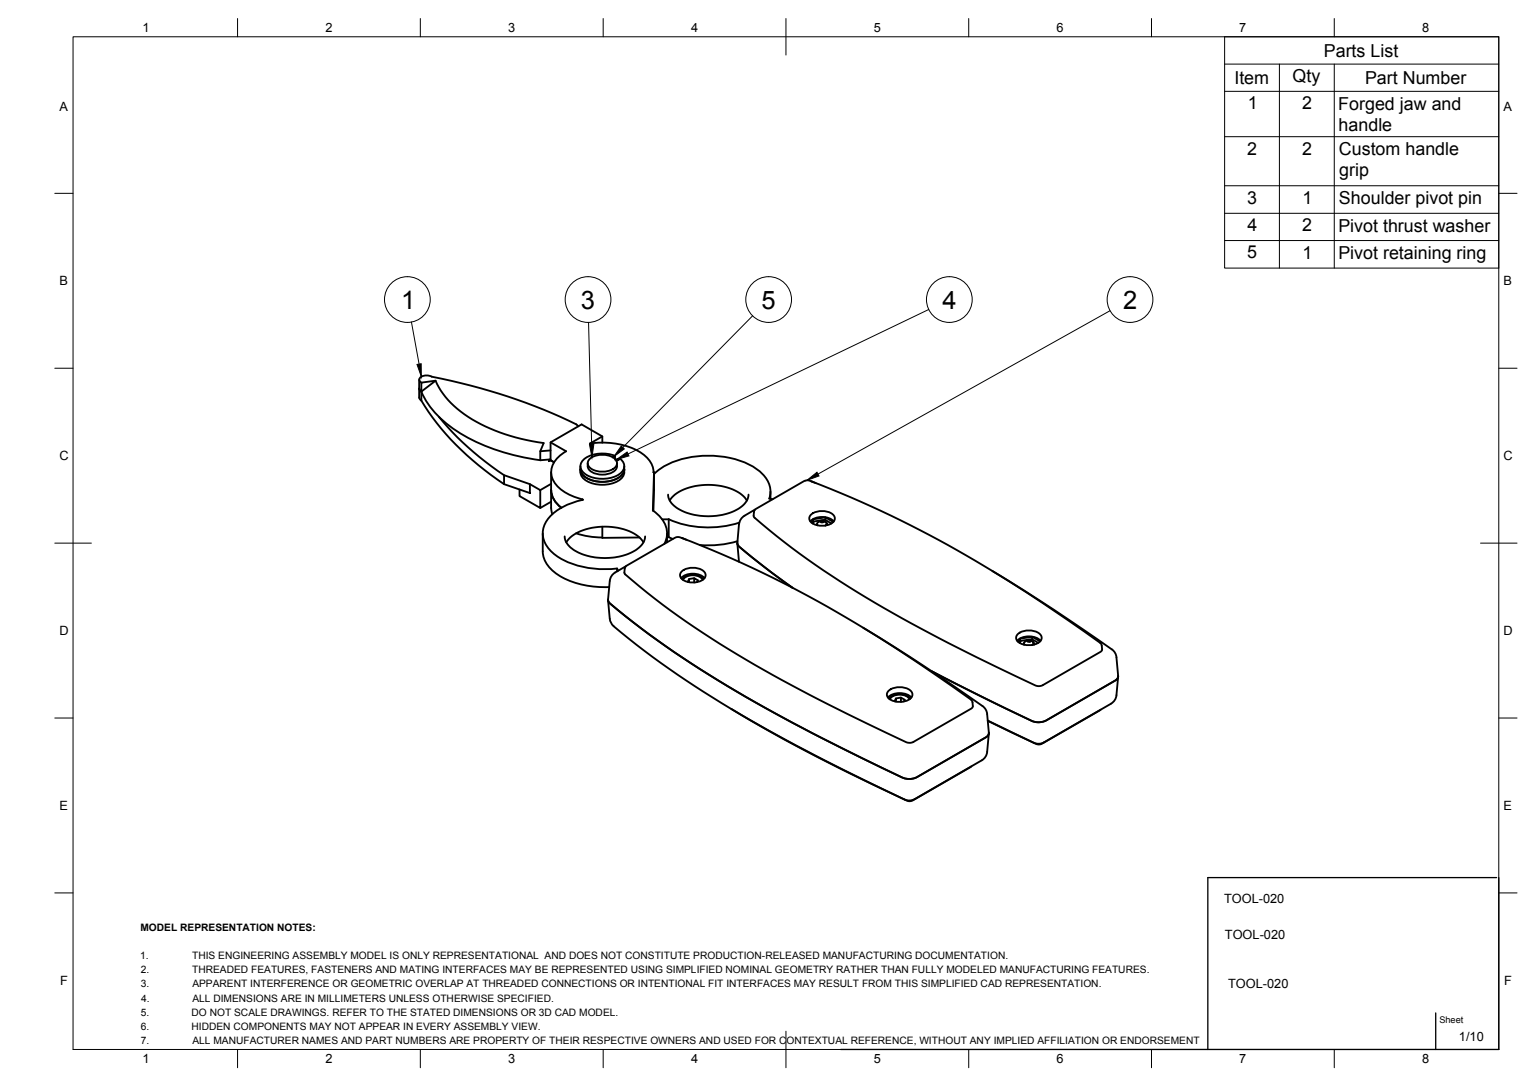
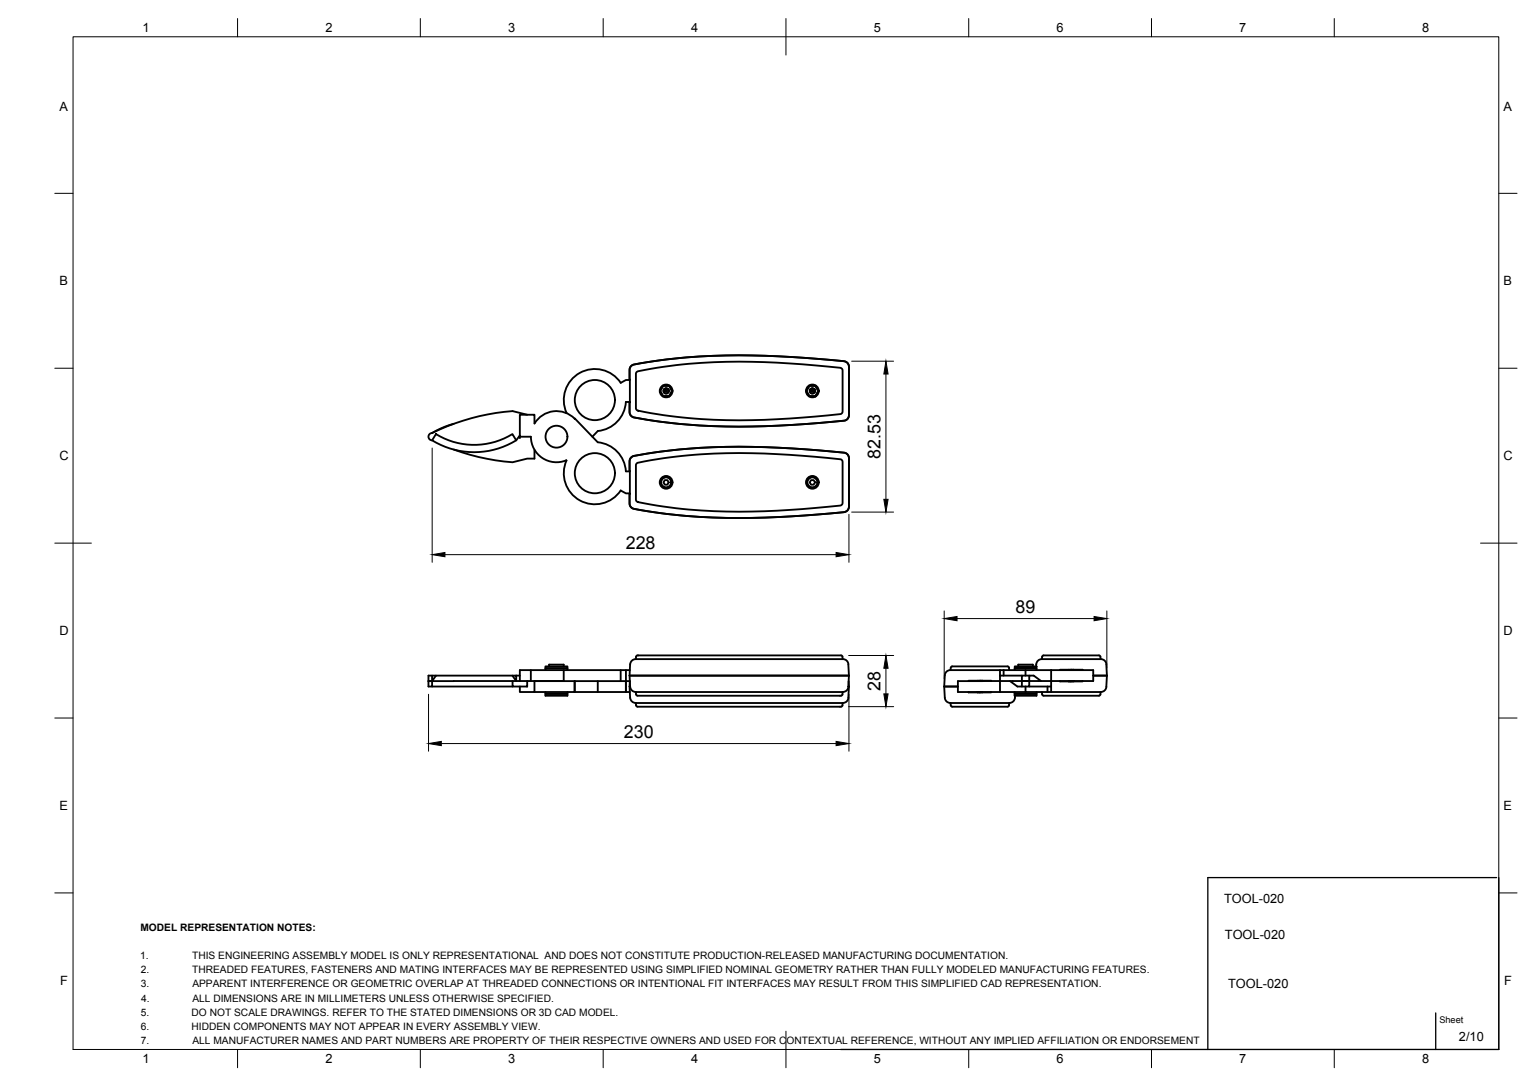
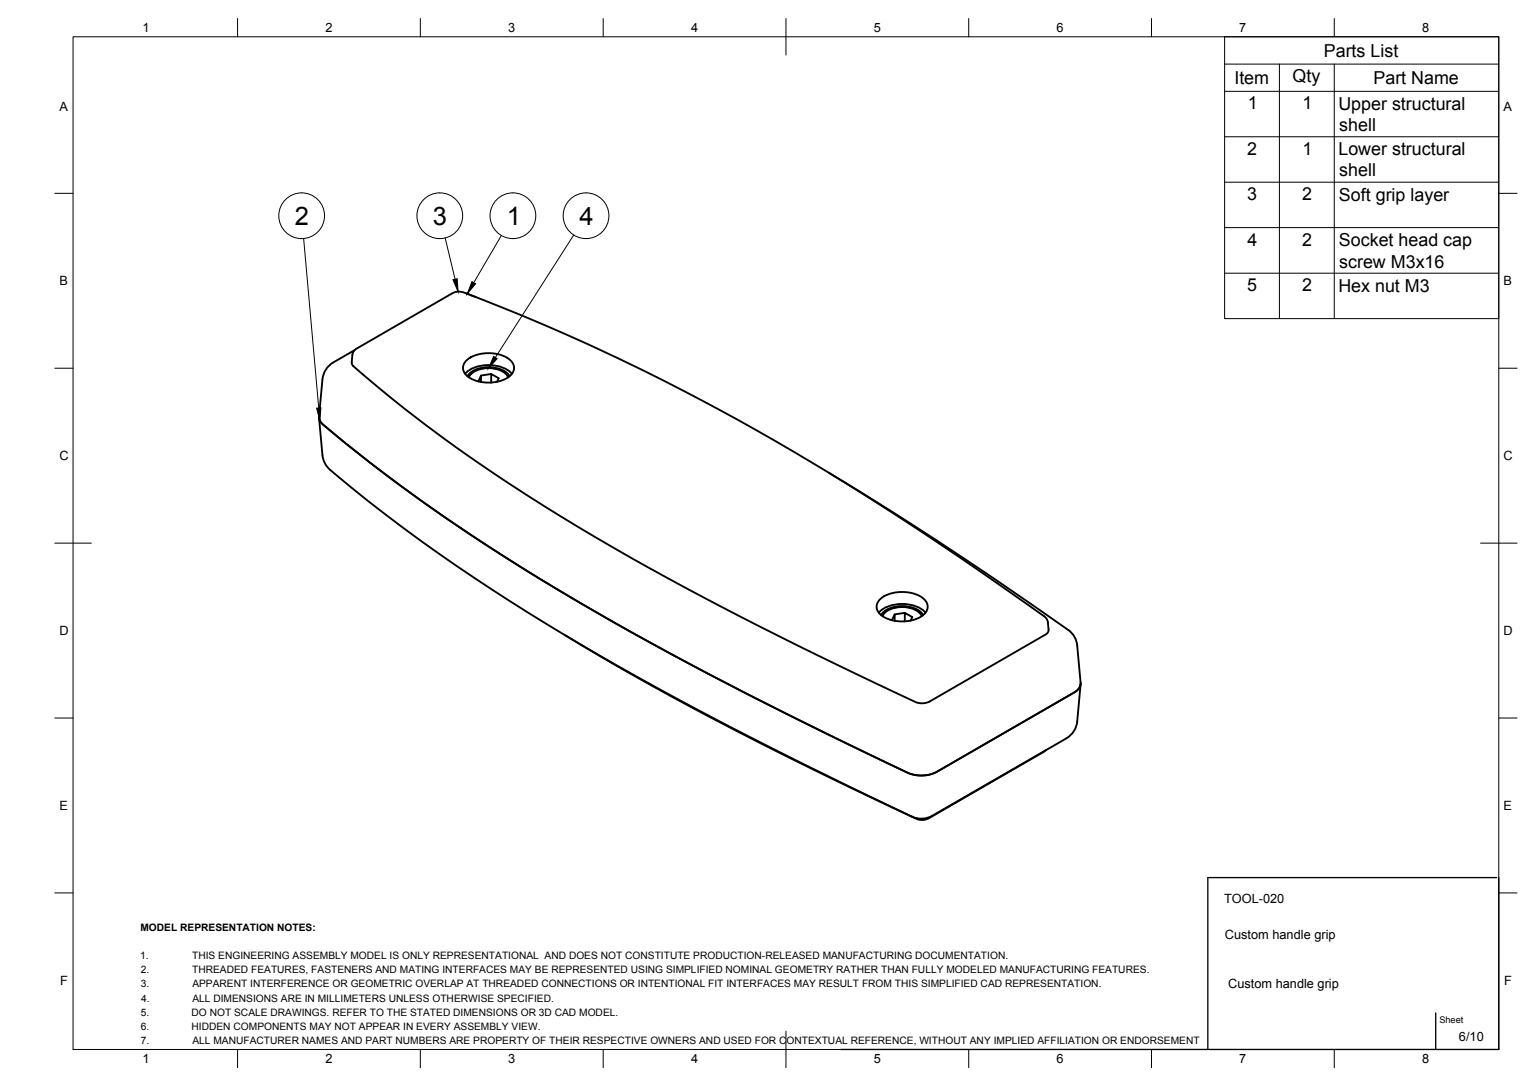
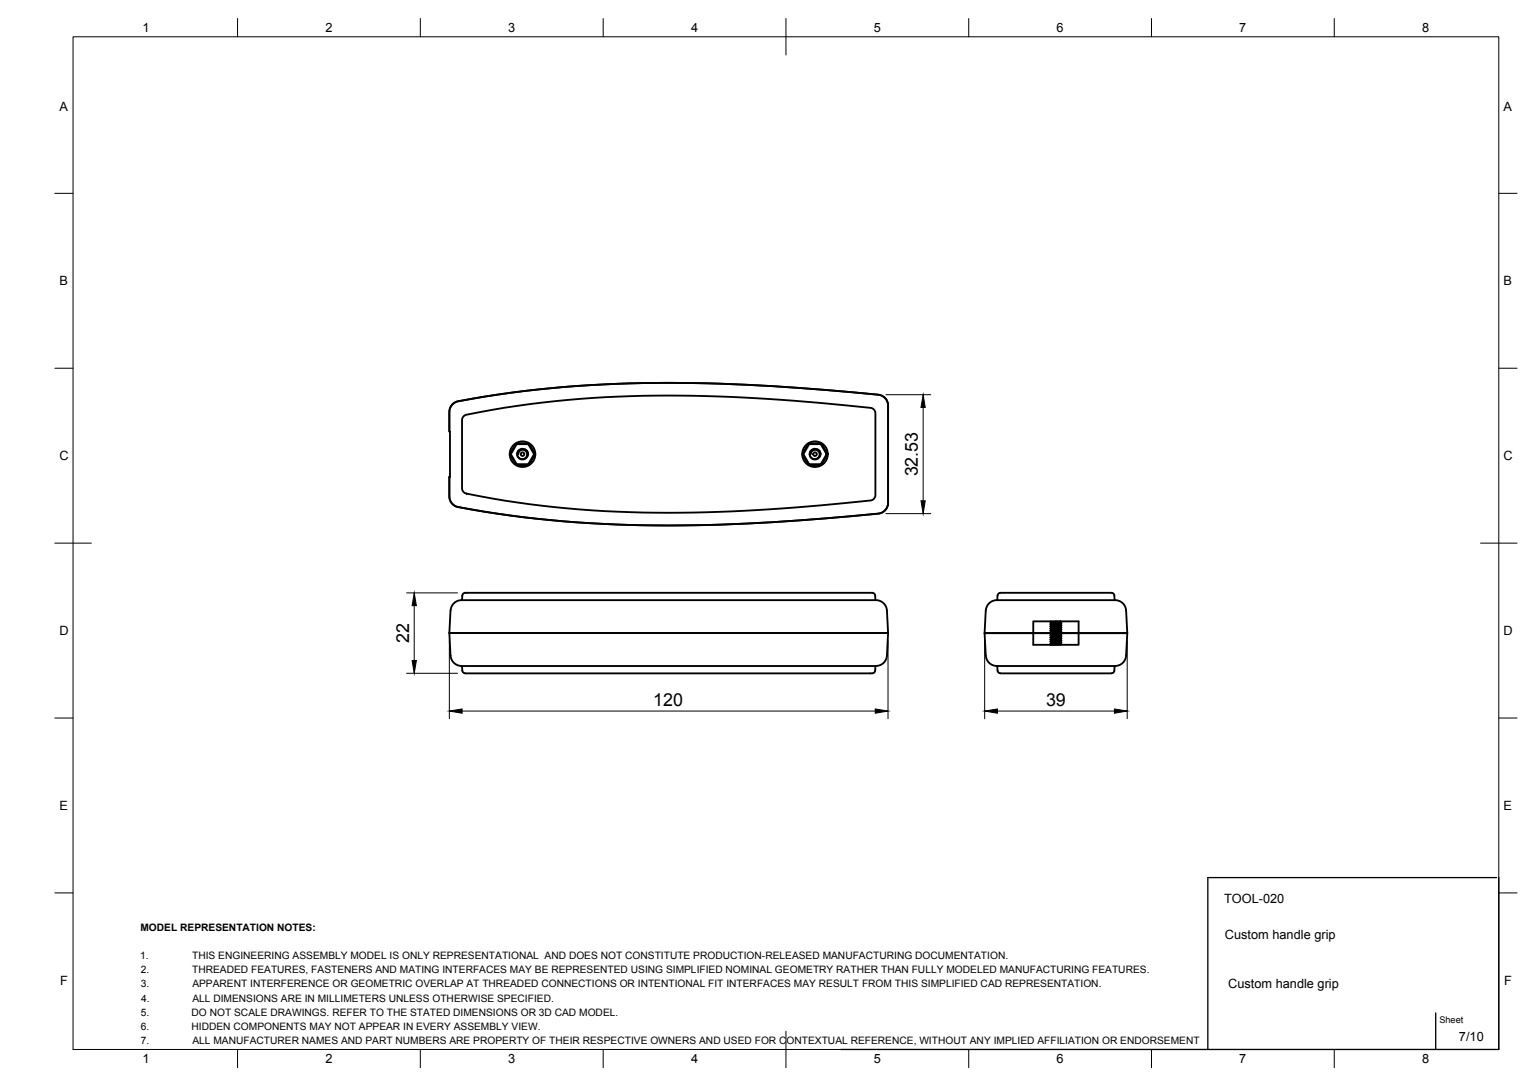
ISO-10303-21;
HEADER;
/* Generated by software containing ST-Developer
 * from STEP Tools, Inc. (www.steptools.com) 
 */

FILE_DESCRIPTION(
/* description */ (''),
/* implementation_level */ '2;1');

FILE_NAME(
/* name */ 'TOOL-020.step',
/* time_stamp */ '2026-11-10T09:09:39-08:00',
/* author */ (''),
/* organization */ (''),
/* preprocessor_version */ 'ST-DEVELOPER v20.2',
/* originating_system */ 'Autodesk Translation Framework v15.17.0.0',
/* authorisation */ '');

FILE_SCHEMA (('AUTOMOTIVE_DESIGN { 1 0 10303 214 3 1 1 }'));
ENDSEC;

DATA;
#10=MECHANICAL_DESIGN_GEOMETRIC_PRESENTATION_REPRESENTATION('',(#555,#556,
#557,#558,#559,#560,#561,#562,#563),#18353);
#11=ITEM_DEFINED_TRANSFORMATION($,$,#6686,#7057);
#12=ITEM_DEFINED_TRANSFORMATION($,$,#6788,#7058);
#13=ITEM_DEFINED_TRANSFORMATION($,$,#6896,#7059);
#14=ITEM_DEFINED_TRANSFORMATION($,$,#6949,#7060);
#15=ITEM_DEFINED_TRANSFORMATION($,$,#7031,#7061);
#16=ITEM_DEFINED_TRANSFORMATION($,$,#6896,#7062);
#17=ITEM_DEFINED_TRANSFORMATION($,$,#6949,#7063);
#18=ITEM_DEFINED_TRANSFORMATION($,$,#7031,#7064);
#19=ITEM_DEFINED_TRANSFORMATION($,$,#6596,#7074);
#20=ITEM_DEFINED_TRANSFORMATION($,$,#6685,#7075);
#21=ITEM_DEFINED_TRANSFORMATION($,$,#6596,#7076);
#22=ITEM_DEFINED_TRANSFORMATION($,$,#6656,#7077);
#23=ITEM_DEFINED_TRANSFORMATION($,$,#7065,#7078);
#24=ITEM_DEFINED_TRANSFORMATION($,$,#6674,#7079);
#25=ITEM_DEFINED_TRANSFORMATION($,$,#6685,#7080);
#26=ITEM_DEFINED_TRANSFORMATION($,$,#7065,#7081);
#27=(
REPRESENTATION_RELATIONSHIP($,$,#18401,#18400)
REPRESENTATION_RELATIONSHIP_WITH_TRANSFORMATION(#11)
SHAPE_REPRESENTATION_RELATIONSHIP()
);
#28=(
REPRESENTATION_RELATIONSHIP($,$,#18402,#18400)
REPRESENTATION_RELATIONSHIP_WITH_TRANSFORMATION(#12)
SHAPE_REPRESENTATION_RELATIONSHIP()
);
#29=(
REPRESENTATION_RELATIONSHIP($,$,#18403,#18400)
REPRESENTATION_RELATIONSHIP_WITH_TRANSFORMATION(#13)
SHAPE_REPRESENTATION_RELATIONSHIP()
);
#30=(
REPRESENTATION_RELATIONSHIP($,$,#18404,#18400)
REPRESENTATION_RELATIONSHIP_WITH_TRANSFORMATION(#14)
SHAPE_REPRESENTATION_RELATIONSHIP()
);
#31=(
REPRESENTATION_RELATIONSHIP($,$,#18405,#18400)
REPRESENTATION_RELATIONSHIP_WITH_TRANSFORMATION(#15)
SHAPE_REPRESENTATION_RELATIONSHIP()
);
#32=(
REPRESENTATION_RELATIONSHIP($,$,#18403,#18400)
REPRESENTATION_RELATIONSHIP_WITH_TRANSFORMATION(#16)
SHAPE_REPRESENTATION_RELATIONSHIP()
);
#33=(
REPRESENTATION_RELATIONSHIP($,$,#18404,#18400)
REPRESENTATION_RELATIONSHIP_WITH_TRANSFORMATION(#17)
SHAPE_REPRESENTATION_RELATIONSHIP()
);
#34=(
REPRESENTATION_RELATIONSHIP($,$,#18405,#18400)
REPRESENTATION_RELATIONSHIP_WITH_TRANSFORMATION(#18)
SHAPE_REPRESENTATION_RELATIONSHIP()
);
#35=(
REPRESENTATION_RELATIONSHIP($,$,#18397,#18396)
REPRESENTATION_RELATIONSHIP_WITH_TRANSFORMATION(#19)
SHAPE_REPRESENTATION_RELATIONSHIP()
);
#36=(
REPRESENTATION_RELATIONSHIP($,$,#18400,#18396)
REPRESENTATION_RELATIONSHIP_WITH_TRANSFORMATION(#20)
SHAPE_REPRESENTATION_RELATIONSHIP()
);
#37=(
REPRESENTATION_RELATIONSHIP($,$,#18397,#18396)
REPRESENTATION_RELATIONSHIP_WITH_TRANSFORMATION(#21)
SHAPE_REPRESENTATION_RELATIONSHIP()
);
#38=(
REPRESENTATION_RELATIONSHIP($,$,#18398,#18396)
REPRESENTATION_RELATIONSHIP_WITH_TRANSFORMATION(#22)
SHAPE_REPRESENTATION_RELATIONSHIP()
);
#39=(
REPRESENTATION_RELATIONSHIP($,$,#18406,#18396)
REPRESENTATION_RELATIONSHIP_WITH_TRANSFORMATION(#23)
SHAPE_REPRESENTATION_RELATIONSHIP()
);
#40=(
REPRESENTATION_RELATIONSHIP($,$,#18399,#18396)
REPRESENTATION_RELATIONSHIP_WITH_TRANSFORMATION(#24)
SHAPE_REPRESENTATION_RELATIONSHIP()
);
#41=(
REPRESENTATION_RELATIONSHIP($,$,#18400,#18396)
REPRESENTATION_RELATIONSHIP_WITH_TRANSFORMATION(#25)
SHAPE_REPRESENTATION_RELATIONSHIP()
);
#42=(
REPRESENTATION_RELATIONSHIP($,$,#18406,#18396)
REPRESENTATION_RELATIONSHIP_WITH_TRANSFORMATION(#26)
SHAPE_REPRESENTATION_RELATIONSHIP()
);
#43=CONTEXT_DEPENDENT_SHAPE_REPRESENTATION(#27,#18379);
#44=CONTEXT_DEPENDENT_SHAPE_REPRESENTATION(#28,#18380);
#45=CONTEXT_DEPENDENT_SHAPE_REPRESENTATION(#29,#18381);
#46=CONTEXT_DEPENDENT_SHAPE_REPRESENTATION(#30,#18382);
#47=CONTEXT_DEPENDENT_SHAPE_REPRESENTATION(#31,#18383);
#48=CONTEXT_DEPENDENT_SHAPE_REPRESENTATION(#32,#18384);
#49=CONTEXT_DEPENDENT_SHAPE_REPRESENTATION(#33,#18385);
#50=CONTEXT_DEPENDENT_SHAPE_REPRESENTATION(#34,#18386);
#51=CONTEXT_DEPENDENT_SHAPE_REPRESENTATION(#35,#18388);
#52=CONTEXT_DEPENDENT_SHAPE_REPRESENTATION(#36,#18389);
#53=CONTEXT_DEPENDENT_SHAPE_REPRESENTATION(#37,#18390);
#54=CONTEXT_DEPENDENT_SHAPE_REPRESENTATION(#38,#18391);
#55=CONTEXT_DEPENDENT_SHAPE_REPRESENTATION(#39,#18392);
#56=CONTEXT_DEPENDENT_SHAPE_REPRESENTATION(#40,#18393);
#57=CONTEXT_DEPENDENT_SHAPE_REPRESENTATION(#41,#18394);
#58=CONTEXT_DEPENDENT_SHAPE_REPRESENTATION(#42,#18395);
#59=NEXT_ASSEMBLY_USAGE_OCCURRENCE('Upper structural shell:1',
'Upper structural shell:1','Upper structural shell:1',#18412,#18413,
'Upper structural shell:1');
#60=NEXT_ASSEMBLY_USAGE_OCCURRENCE('Lower structural shell:1',
'Lower structural shell:1','Lower structural shell:1',#18412,#18414,
'Lower structural shell:1');
#61=NEXT_ASSEMBLY_USAGE_OCCURRENCE('Soft grip layer:1',
'Soft grip layer:1','Soft grip layer:1',#18412,#18415,
'Soft grip layer:1');
#62=NEXT_ASSEMBLY_USAGE_OCCURRENCE('Socket head cap screw M3x16:1',
'Socket head cap screw M3x16:1','Socket head cap screw M3x16:1',#18412,
#18416,'Socket head cap screw M3x16:1');
#63=NEXT_ASSEMBLY_USAGE_OCCURRENCE('Hex nut M3:1','Hex nut M3:1',
'Hex nut M3:1',#18412,#18417,'Hex nut M3:1');
#64=NEXT_ASSEMBLY_USAGE_OCCURRENCE('Soft grip layer:2',
'Soft grip layer:2','Soft grip layer:2',#18412,#18415,
'Soft grip layer:2');
#65=NEXT_ASSEMBLY_USAGE_OCCURRENCE('Socket head cap screw M3x16:2',
'Socket head cap screw M3x16:2','Socket head cap screw M3x16:2',#18412,
#18416,'Socket head cap screw M3x16:2');
#66=NEXT_ASSEMBLY_USAGE_OCCURRENCE('Hex nut M3:2','Hex nut M3:2',
'Hex nut M3:2',#18412,#18417,'Hex nut M3:2');
#67=NEXT_ASSEMBLY_USAGE_OCCURRENCE('Forged jaw and handle:1',
'Forged jaw and handle:1','Forged jaw and handle:1',#18408,#18409,
'Forged jaw and handle:1');
#68=NEXT_ASSEMBLY_USAGE_OCCURRENCE('Custom handle grip:1',
'Custom handle grip:1','Custom handle grip:1',#18408,#18412,
'Custom handle grip:1');
#69=NEXT_ASSEMBLY_USAGE_OCCURRENCE('Forged jaw and handle:2',
'Forged jaw and handle:2','Forged jaw and handle:2',#18408,#18409,
'Forged jaw and handle:2');
#70=NEXT_ASSEMBLY_USAGE_OCCURRENCE('Shoulder pivot pin:1',
'Shoulder pivot pin:1','Shoulder pivot pin:1',#18408,#18410,
'Shoulder pivot pin:1');
#71=NEXT_ASSEMBLY_USAGE_OCCURRENCE('Pivot thrust washer:1',
'Pivot thrust washer:1','Pivot thrust washer:1',#18408,#18418,
'Pivot thrust washer:1');
#72=NEXT_ASSEMBLY_USAGE_OCCURRENCE('Pivot retaining ring:1',
'Pivot retaining ring:1','Pivot retaining ring:1',#18408,#18411,
'Pivot retaining ring:1');
#73=NEXT_ASSEMBLY_USAGE_OCCURRENCE('Custom handle grip:2',
'Custom handle grip:2','Custom handle grip:2',#18408,#18412,
'Custom handle grip:2');
#74=NEXT_ASSEMBLY_USAGE_OCCURRENCE('Pivot thrust washer:2',
'Pivot thrust washer:2','Pivot thrust washer:2',#18408,#18418,
'Pivot thrust washer:2');
#75=SPHERICAL_SURFACE('',#6751,0.0999999999999999);
#76=SPHERICAL_SURFACE('',#6754,0.100000000000002);
#77=SPHERICAL_SURFACE('',#6758,0.0999999999999991);
#78=SPHERICAL_SURFACE('',#6762,0.1);
#79=SPHERICAL_SURFACE('',#6767,0.3);
#80=SPHERICAL_SURFACE('',#6771,0.300000000000002);
#81=SPHERICAL_SURFACE('',#6775,0.299999999999999);
#82=SPHERICAL_SURFACE('',#6780,0.3);
#83=SPHERICAL_SURFACE('',#6859,0.0999999999999999);
#84=SPHERICAL_SURFACE('',#6862,0.100000000000002);
#85=SPHERICAL_SURFACE('',#6866,0.0999999999999991);
#86=SPHERICAL_SURFACE('',#6870,0.1);
#87=SPHERICAL_SURFACE('',#6875,0.3);
#88=SPHERICAL_SURFACE('',#6879,0.300000000000002);
#89=SPHERICAL_SURFACE('',#6883,0.299999999999999);
#90=SPHERICAL_SURFACE('',#6888,0.3);
#91=B_SPLINE_SURFACE_WITH_KNOTS('',3,3,((#9570,#9571,#9572,#9573),(#9574,
#9575,#9576,#9577),(#9578,#9579,#9580,#9581),(#9582,#9583,#9584,#9585)),
 .UNSPECIFIED.,.F.,.F.,.F.,(4,4),(4,4),(0.0627625298587661,0.3242096015809),
(0.0118073085896899,0.685451490706028),.UNSPECIFIED.);
#92=B_SPLINE_SURFACE_WITH_KNOTS('',3,3,((#9590,#9591,#9592,#9593),(#9594,
#9595,#9596,#9597),(#9598,#9599,#9600,#9601),(#9602,#9603,#9604,#9605)),
 .UNSPECIFIED.,.F.,.F.,.F.,(4,4),(4,4),(0.0225360950145449,0.0483865590996774),
(0.0125659096559557,0.685650832343257),.UNSPECIFIED.);
#93=B_SPLINE_SURFACE_WITH_KNOTS('',3,3,((#9615,#9616,#9617,#9618),(#9619,
#9620,#9621,#9622),(#9623,#9624,#9625,#9626),(#9627,#9628,#9629,#9630),
(#9631,#9632,#9633,#9634)),.UNSPECIFIED.,.F.,.F.,.F.,(4,1,4),(4,4),(0.,
0.571428571428571,1.),(0.74118252158834,3.85438678954986),.UNSPECIFIED.);
#94=B_SPLINE_SURFACE_WITH_KNOTS('',3,3,((#9639,#9640,#9641,#9642),(#9643,
#9644,#9645,#9646),(#9647,#9648,#9649,#9650),(#9651,#9652,#9653,#9654),
(#9655,#9656,#9657,#9658)),.UNSPECIFIED.,.F.,.F.,.F.,(4,1,4),(4,4),(0.,
0.571428571428571,1.),(0.270878787657975,0.54981857912664),
 .UNSPECIFIED.);
#95=B_SPLINE_SURFACE_WITH_KNOTS('',3,3,((#9677,#9678,#9679,#9680),(#9681,
#9682,#9683,#9684),(#9685,#9686,#9687,#9688),(#9689,#9690,#9691,#9692),
(#9693,#9694,#9695,#9696)),.UNSPECIFIED.,.F.,.F.,.F.,(4,1,4),(4,4),(0.,
0.571428571428571,1.),(8.03948512627517,11.1526893942367),.UNSPECIFIED.);
#96=B_SPLINE_SURFACE_WITH_KNOTS('',3,3,((#9701,#9702,#9703,#9704),(#9705,
#9706,#9707,#9708),(#9709,#9710,#9711,#9712),(#9713,#9714,#9715,#9716)),
 .UNSPECIFIED.,.F.,.F.,.F.,(4,4),(4,4),(0.675790398419059,0.937237470141233),
(0.0118073085603101,0.685451490706029),.UNSPECIFIED.);
#97=B_SPLINE_SURFACE_WITH_KNOTS('',3,3,((#9717,#9718,#9719,#9720),(#9721,
#9722,#9723,#9724),(#9725,#9726,#9727,#9728),(#9729,#9730,#9731,#9732)),
 .UNSPECIFIED.,.F.,.F.,.F.,(4,4),(4,4),(0.951613440900322,0.977463904985455),
(0.0125659096559558,0.685650832343257),.UNSPECIFIED.);
#98=B_SPLINE_SURFACE_WITH_KNOTS('',3,3,((#9816,#9817,#9818,#9819),(#9820,
#9821,#9822,#9823),(#9824,#9825,#9826,#9827),(#9828,#9829,#9830,#9831)),
 .UNSPECIFIED.,.F.,.F.,.F.,(4,4),(4,4),(0.340089900275858,0.660082688299826),
(0.0116294244283504,0.684384408933581),.UNSPECIFIED.);
#99=B_SPLINE_SURFACE_WITH_KNOTS('',3,3,((#9836,#9837,#9838,#9839),(#9840,
#9841,#9842,#9843),(#9844,#9845,#9846,#9847),(#9848,#9849,#9850,#9851),
(#9852,#9853,#9854,#9855)),.UNSPECIFIED.,.F.,.F.,.F.,(4,1,4),(4,4),(0.,
0.571428571428571,1.),(4.04989375377528,7.85140214144331),.UNSPECIFIED.);
#100=B_SPLINE_SURFACE_WITH_KNOTS('',3,3,((#9865,#9866,#9867,#9868),(#9869,
#9870,#9871,#9872),(#9873,#9874,#9875,#9876),(#9877,#9878,#9879,#9880),
(#9881,#9882,#9883,#9884)),.UNSPECIFIED.,.F.,.F.,.F.,(4,1,4),(4,4),(0.,
0.571428571428571,1.),(4.0424697743818,7.84397816204974),.UNSPECIFIED.);
#101=B_SPLINE_SURFACE_WITH_KNOTS('',3,3,((#9889,#9890,#9891,#9892),(#9893,
#9894,#9895,#9896),(#9897,#9898,#9899,#9900),(#9901,#9902,#9903,#9904)),
 .UNSPECIFIED.,.F.,.F.,.F.,(4,4),(4,4),(0.339917311700174,0.659910099724142),
(0.0116294573698948,0.684384408933581),.UNSPECIFIED.);
#102=B_SPLINE_SURFACE_WITH_KNOTS('',3,3,((#9979,#9980,#9981,#9982),(#9983,
#9984,#9985,#9986),(#9987,#9988,#9989,#9990),(#9991,#9992,#9993,#9994)),
 .UNSPECIFIED.,.F.,.F.,.F.,(4,4),(4,4),(0.675996615945502,0.913173856075534),
(0.0118505108223707,0.686152089762332),.UNSPECIFIED.);
#103=B_SPLINE_SURFACE_WITH_KNOTS('',3,3,((#9999,#10000,#10001,#10002),(#10003,
#10004,#10005,#10006),(#10007,#10008,#10009,#10010),(#10011,#10012,#10013,
#10014),(#10015,#10016,#10017,#10018)),.UNSPECIFIED.,.F.,.F.,.F.,(4,1,4),
(4,4),(0.,0.571428571428571,1.),(8.0457708503995,10.8690635835914),
 .UNSPECIFIED.);
#104=B_SPLINE_SURFACE_WITH_KNOTS('',3,3,((#10028,#10029,#10030,#10031),
(#10032,#10033,#10034,#10035),(#10036,#10037,#10038,#10039),(#10040,#10041,
#10042,#10043),(#10044,#10045,#10046,#10047)),.UNSPECIFIED.,.F.,.F.,.F.,
(4,1,4),(4,4),(0.,0.571428571428571,1.),(1.02480833223363,3.8481010654256),
 .UNSPECIFIED.);
#105=B_SPLINE_SURFACE_WITH_KNOTS('',3,3,((#10052,#10053,#10054,#10055),
(#10056,#10057,#10058,#10059),(#10060,#10061,#10062,#10063),(#10064,#10065,
#10066,#10067)),.UNSPECIFIED.,.F.,.F.,.F.,(4,4),(4,4),(0.0868261439244655,
0.324003384054498),(0.0118505108223707,0.686152089762332),.UNSPECIFIED.);
#106=B_SPLINE_SURFACE_WITH_KNOTS('',3,3,((#10142,#10143,#10144,#10145),
(#10146,#10147,#10148,#10149),(#10150,#10151,#10152,#10153),(#10154,#10155,
#10156,#10157)),.UNSPECIFIED.,.F.,.F.,.F.,(4,4),(4,4),(0.927751606342899,
0.979699913047832),(0.0130895688562318,0.686930956013783),.UNSPECIFIED.);
#107=B_SPLINE_SURFACE_WITH_KNOTS('',3,3,((#10167,#10168,#10169,#10170),
(#10171,#10172,#10173,#10174),(#10175,#10176,#10177,#10178),(#10179,#10180,
#10181,#10182),(#10183,#10184,#10185,#10186)),.UNSPECIFIED.,.F.,.F.,.F.,
(4,1,4),(4,4),(0.,0.571428571428571,1.),(11.0550486447215,11.6488871259622),
 .UNSPECIFIED.);
#108=B_SPLINE_SURFACE_WITH_KNOTS('',3,3,((#10200,#10201,#10202,#10203),
(#10204,#10205,#10206,#10207),(#10208,#10209,#10210,#10211),(#10212,#10213,
#10214,#10215)),.UNSPECIFIED.,.F.,.F.,.F.,(4,4),(4,4),(0.0203000869521683,
0.0722483936571013),(0.0130895688562318,0.686930956013783),
 .UNSPECIFIED.);
#109=B_SPLINE_SURFACE_WITH_KNOTS('',3,3,((#10225,#10226,#10227,#10228),
(#10229,#10230,#10231,#10232),(#10233,#10234,#10235,#10236),(#10237,#10238,
#10239,#10240),(#10241,#10242,#10243,#10244)),.UNSPECIFIED.,.F.,.F.,.F.,
(4,1,4),(4,4),(0.,0.571428571428571,1.),(0.244984789862841,0.838823271103535),
 .UNSPECIFIED.);
#110=B_SPLINE_SURFACE_WITH_KNOTS('',3,3,((#10258,#10259,#10260,#10261),
(#10262,#10263,#10264,#10265),(#10266,#10267,#10268,#10269),(#10270,#10271,
#10272,#10273),(#10274,#10275,#10276,#10277)),.UNSPECIFIED.,.F.,.F.,.F.,
(4,1,4),(4,4),(0.,0.5,1.),(0.0108921325678979,0.619909717328002),
 .UNSPECIFIED.);
#111=B_SPLINE_SURFACE_WITH_KNOTS('',3,3,((#10284,#10285,#10286,#10287),
(#10288,#10289,#10290,#10291),(#10292,#10293,#10294,#10295),(#10296,#10297,
#10298,#10299),(#10300,#10301,#10302,#10303)),.UNSPECIFIED.,.F.,.F.,.F.,
(4,1,4),(4,4),(0.,0.571428571428571,1.),(0.00967450486392679,0.618764321025346),
 .UNSPECIFIED.);
#112=B_SPLINE_SURFACE_WITH_KNOTS('',3,3,((#10308,#10309,#10310,#10311),
(#10312,#10313,#10314,#10315),(#10316,#10317,#10318,#10319),(#10320,#10321,
#10322,#10323),(#10324,#10325,#10326,#10327)),.UNSPECIFIED.,.F.,.F.,.F.,
(4,1,4),(4,4),(0.,0.571428571428571,1.),(0.0097274579809394,0.618764321025346),
 .UNSPECIFIED.);
#113=B_SPLINE_SURFACE_WITH_KNOTS('',3,3,((#10332,#10333,#10334,#10335),
(#10336,#10337,#10338,#10339),(#10340,#10341,#10342,#10343),(#10344,#10345,
#10346,#10347),(#10348,#10349,#10350,#10351)),.UNSPECIFIED.,.F.,.F.,.F.,
(4,1,4),(4,4),(0.,0.571428571428571,1.),(11.3440533366984,11.6229931281671),
 .UNSPECIFIED.);
#114=B_SPLINE_SURFACE_WITH_KNOTS('',3,3,((#10352,#10353,#10354,#10355),
(#10356,#10357,#10358,#10359),(#10360,#10361,#10362,#10363),(#10364,#10365,
#10366,#10367),(#10368,#10369,#10370,#10371)),.UNSPECIFIED.,.F.,.F.,.F.,
(4,1,4),(4,4),(0.,0.5,1.),(0.0108402259132964,0.619909717328002),
 .UNSPECIFIED.);
#115=B_SPLINE_SURFACE_WITH_KNOTS('',3,3,((#10397,#10398,#10399,#10400),
(#10401,#10402,#10403,#10404),(#10405,#10406,#10407,#10408),(#10409,#10410,
#10411,#10412),(#10413,#10414,#10415,#10416)),.UNSPECIFIED.,.F.,.F.,.F.,
(4,1,4),(4,4),(0.,0.571428571428571,1.),(-0.00387706229521417,0.619909717328002),
 .UNSPECIFIED.);
#116=B_SPLINE_SURFACE_WITH_KNOTS('',3,3,((#10435,#10436,#10437,#10438,#10439,
#10440),(#10441,#10442,#10443,#10444,#10445,#10446),(#10447,#10448,#10449,
#10450,#10451,#10452),(#10453,#10454,#10455,#10456,#10457,#10458),(#10459,
#10460,#10461,#10462,#10463,#10464)),.UNSPECIFIED.,.F.,.F.,.F.,(4,1,4),
(4,1,1,4),(0.,0.571428571428571,1.),(0.270878787657975,5.14716807550265,
8.39802760073243,11.6488871259622),.UNSPECIFIED.);
#117=B_SPLINE_SURFACE_WITH_KNOTS('',3,3,((#10477,#10478,#10479,#10480),
(#10481,#10482,#10483,#10484),(#10485,#10486,#10487,#10488),(#10489,#10490,
#10491,#10492),(#10493,#10494,#10495,#10496)),.UNSPECIFIED.,.F.,.F.,.F.,
(4,1,4),(4,4),(0.,0.571428571428571,1.),(-0.00522825793187074,0.618764321025346),
 .UNSPECIFIED.);
#118=B_SPLINE_SURFACE_WITH_KNOTS('',3,3,((#10505,#10506,#10507,#10508),
(#10509,#10510,#10511,#10512),(#10513,#10514,#10515,#10516),(#10517,#10518,
#10519,#10520),(#10521,#10522,#10523,#10524)),.UNSPECIFIED.,.F.,.F.,.F.,
(4,1,4),(4,4),(0.,0.571428571428571,1.),(-0.00506942997988007,0.618764321025346),
 .UNSPECIFIED.);
#119=B_SPLINE_SURFACE_WITH_KNOTS('',3,3,((#10533,#10534,#10535,#10536,#10537),
(#10538,#10539,#10540,#10541,#10542),(#10543,#10544,#10545,#10546,#10547),
(#10548,#10549,#10550,#10551,#10552),(#10553,#10554,#10555,#10556,#10557)),
 .UNSPECIFIED.,.F.,.F.,.F.,(4,1,4),(4,1,4),(0.,0.571428571428571,1.),(0.244984789862841,
5.12127407770751,11.6229931281671),.UNSPECIFIED.);
#120=B_SPLINE_SURFACE_WITH_KNOTS('',3,3,((#10568,#10569,#10570,#10571),
(#10572,#10573,#10574,#10575),(#10576,#10577,#10578,#10579),(#10580,#10581,
#10582,#10583),(#10584,#10585,#10586,#10587)),.UNSPECIFIED.,.F.,.F.,.F.,
(4,1,4),(4,4),(0.,0.571428571428571,1.),(-0.00403278922781227,0.619909717328002),
 .UNSPECIFIED.);
#121=B_SPLINE_SURFACE_WITH_KNOTS('',3,3,((#10596,#10597,#10598,#10599),
(#10600,#10601,#10602,#10603),(#10604,#10605,#10606,#10607),(#10608,#10609,
#10610,#10611)),.UNSPECIFIED.,.F.,.F.,.F.,(4,4),(4,4),(0.0225340877622934,
0.979701609653785),(0.,0.686930956013783),.UNSPECIFIED.);
#122=B_SPLINE_SURFACE_WITH_KNOTS('',3,3,((#10614,#10615,#10616,#10617),
(#10618,#10619,#10620,#10621),(#10622,#10623,#10624,#10625),(#10626,#10627,
#10628,#10629)),.UNSPECIFIED.,.F.,.F.,.F.,(4,4),(4,4),(0.0202983903462145,
0.977465912237707),(0.,0.686930956013783),.UNSPECIFIED.);
#123=B_SPLINE_SURFACE_WITH_KNOTS('',3,3,((#11565,#11566,#11567,#11568),
(#11569,#11570,#11571,#11572),(#11573,#11574,#11575,#11576),(#11577,#11578,
#11579,#11580)),.UNSPECIFIED.,.F.,.F.,.F.,(4,4),(4,4),(0.0627625298587661,
0.3242096015809),(0.0118073085896899,0.685451490706028),.UNSPECIFIED.);
#124=B_SPLINE_SURFACE_WITH_KNOTS('',3,3,((#11585,#11586,#11587,#11588),
(#11589,#11590,#11591,#11592),(#11593,#11594,#11595,#11596),(#11597,#11598,
#11599,#11600)),.UNSPECIFIED.,.F.,.F.,.F.,(4,4),(4,4),(0.0225360950145449,
0.0483865590996774),(0.0125659096559557,0.685650832343257),
 .UNSPECIFIED.);
#125=B_SPLINE_SURFACE_WITH_KNOTS('',3,3,((#11610,#11611,#11612,#11613),
(#11614,#11615,#11616,#11617),(#11618,#11619,#11620,#11621),(#11622,#11623,
#11624,#11625),(#11626,#11627,#11628,#11629)),.UNSPECIFIED.,.F.,.F.,.F.,
(4,1,4),(4,4),(0.,0.571428571428571,1.),(0.74118252158834,3.85438678954986),
 .UNSPECIFIED.);
#126=B_SPLINE_SURFACE_WITH_KNOTS('',3,3,((#11634,#11635,#11636,#11637),
(#11638,#11639,#11640,#11641),(#11642,#11643,#11644,#11645),(#11646,#11647,
#11648,#11649),(#11650,#11651,#11652,#11653)),.UNSPECIFIED.,.F.,.F.,.F.,
(4,1,4),(4,4),(0.,0.571428571428571,1.),(0.270878787657975,0.54981857912664),
 .UNSPECIFIED.);
#127=B_SPLINE_SURFACE_WITH_KNOTS('',3,3,((#11672,#11673,#11674,#11675),
(#11676,#11677,#11678,#11679),(#11680,#11681,#11682,#11683),(#11684,#11685,
#11686,#11687),(#11688,#11689,#11690,#11691)),.UNSPECIFIED.,.F.,.F.,.F.,
(4,1,4),(4,4),(0.,0.571428571428571,1.),(8.03948512627517,11.1526893942367),
 .UNSPECIFIED.);
#128=B_SPLINE_SURFACE_WITH_KNOTS('',3,3,((#11696,#11697,#11698,#11699),
(#11700,#11701,#11702,#11703),(#11704,#11705,#11706,#11707),(#11708,#11709,
#11710,#11711)),.UNSPECIFIED.,.F.,.F.,.F.,(4,4),(4,4),(0.675790398419059,
0.937237470141233),(0.0118073085603101,0.685451490706029),.UNSPECIFIED.);
#129=B_SPLINE_SURFACE_WITH_KNOTS('',3,3,((#11712,#11713,#11714,#11715),
(#11716,#11717,#11718,#11719),(#11720,#11721,#11722,#11723),(#11724,#11725,
#11726,#11727)),.UNSPECIFIED.,.F.,.F.,.F.,(4,4),(4,4),(0.951613440900322,
0.977463904985455),(0.0125659096559558,0.685650832343257),.UNSPECIFIED.);
#130=B_SPLINE_SURFACE_WITH_KNOTS('',3,3,((#11811,#11812,#11813,#11814),
(#11815,#11816,#11817,#11818),(#11819,#11820,#11821,#11822),(#11823,#11824,
#11825,#11826)),.UNSPECIFIED.,.F.,.F.,.F.,(4,4),(4,4),(0.340089900275858,
0.660082688299826),(0.0116294244283504,0.684384408933581),.UNSPECIFIED.);
#131=B_SPLINE_SURFACE_WITH_KNOTS('',3,3,((#11831,#11832,#11833,#11834),
(#11835,#11836,#11837,#11838),(#11839,#11840,#11841,#11842),(#11843,#11844,
#11845,#11846),(#11847,#11848,#11849,#11850)),.UNSPECIFIED.,.F.,.F.,.F.,
(4,1,4),(4,4),(0.,0.571428571428571,1.),(4.04989375377528,7.85140214144331),
 .UNSPECIFIED.);
#132=B_SPLINE_SURFACE_WITH_KNOTS('',3,3,((#11860,#11861,#11862,#11863),
(#11864,#11865,#11866,#11867),(#11868,#11869,#11870,#11871),(#11872,#11873,
#11874,#11875),(#11876,#11877,#11878,#11879)),.UNSPECIFIED.,.F.,.F.,.F.,
(4,1,4),(4,4),(0.,0.571428571428571,1.),(4.0424697743818,7.84397816204974),
 .UNSPECIFIED.);
#133=B_SPLINE_SURFACE_WITH_KNOTS('',3,3,((#11884,#11885,#11886,#11887),
(#11888,#11889,#11890,#11891),(#11892,#11893,#11894,#11895),(#11896,#11897,
#11898,#11899)),.UNSPECIFIED.,.F.,.F.,.F.,(4,4),(4,4),(0.339917311700174,
0.659910099724142),(0.0116294573698948,0.684384408933581),.UNSPECIFIED.);
#134=B_SPLINE_SURFACE_WITH_KNOTS('',3,3,((#11974,#11975,#11976,#11977),
(#11978,#11979,#11980,#11981),(#11982,#11983,#11984,#11985),(#11986,#11987,
#11988,#11989)),.UNSPECIFIED.,.F.,.F.,.F.,(4,4),(4,4),(0.675996615945502,
0.913173856075534),(0.0118505108223707,0.686152089762332),.UNSPECIFIED.);
#135=B_SPLINE_SURFACE_WITH_KNOTS('',3,3,((#11994,#11995,#11996,#11997),
(#11998,#11999,#12000,#12001),(#12002,#12003,#12004,#12005),(#12006,#12007,
#12008,#12009),(#12010,#12011,#12012,#12013)),.UNSPECIFIED.,.F.,.F.,.F.,
(4,1,4),(4,4),(0.,0.571428571428571,1.),(8.0457708503995,10.8690635835914),
 .UNSPECIFIED.);
#136=B_SPLINE_SURFACE_WITH_KNOTS('',3,3,((#12023,#12024,#12025,#12026),
(#12027,#12028,#12029,#12030),(#12031,#12032,#12033,#12034),(#12035,#12036,
#12037,#12038),(#12039,#12040,#12041,#12042)),.UNSPECIFIED.,.F.,.F.,.F.,
(4,1,4),(4,4),(0.,0.571428571428571,1.),(1.02480833223363,3.8481010654256),
 .UNSPECIFIED.);
#137=B_SPLINE_SURFACE_WITH_KNOTS('',3,3,((#12047,#12048,#12049,#12050),
(#12051,#12052,#12053,#12054),(#12055,#12056,#12057,#12058),(#12059,#12060,
#12061,#12062)),.UNSPECIFIED.,.F.,.F.,.F.,(4,4),(4,4),(0.0868261439244655,
0.324003384054498),(0.0118505108223707,0.686152089762332),.UNSPECIFIED.);
#138=B_SPLINE_SURFACE_WITH_KNOTS('',3,3,((#12137,#12138,#12139,#12140),
(#12141,#12142,#12143,#12144),(#12145,#12146,#12147,#12148),(#12149,#12150,
#12151,#12152)),.UNSPECIFIED.,.F.,.F.,.F.,(4,4),(4,4),(0.927751606342899,
0.979699913047832),(0.0130895688562318,0.686930956013783),.UNSPECIFIED.);
#139=B_SPLINE_SURFACE_WITH_KNOTS('',3,3,((#12162,#12163,#12164,#12165),
(#12166,#12167,#12168,#12169),(#12170,#12171,#12172,#12173),(#12174,#12175,
#12176,#12177),(#12178,#12179,#12180,#12181)),.UNSPECIFIED.,.F.,.F.,.F.,
(4,1,4),(4,4),(0.,0.571428571428571,1.),(11.0550486447215,11.6488871259622),
 .UNSPECIFIED.);
#140=B_SPLINE_SURFACE_WITH_KNOTS('',3,3,((#12195,#12196,#12197,#12198),
(#12199,#12200,#12201,#12202),(#12203,#12204,#12205,#12206),(#12207,#12208,
#12209,#12210)),.UNSPECIFIED.,.F.,.F.,.F.,(4,4),(4,4),(0.0203000869521683,
0.0722483936571013),(0.0130895688562318,0.686930956013783),
 .UNSPECIFIED.);
#141=B_SPLINE_SURFACE_WITH_KNOTS('',3,3,((#12220,#12221,#12222,#12223),
(#12224,#12225,#12226,#12227),(#12228,#12229,#12230,#12231),(#12232,#12233,
#12234,#12235),(#12236,#12237,#12238,#12239)),.UNSPECIFIED.,.F.,.F.,.F.,
(4,1,4),(4,4),(0.,0.571428571428571,1.),(0.244984789862841,0.838823271103535),
 .UNSPECIFIED.);
#142=B_SPLINE_SURFACE_WITH_KNOTS('',3,3,((#12253,#12254,#12255,#12256),
(#12257,#12258,#12259,#12260),(#12261,#12262,#12263,#12264),(#12265,#12266,
#12267,#12268),(#12269,#12270,#12271,#12272)),.UNSPECIFIED.,.F.,.F.,.F.,
(4,1,4),(4,4),(0.,0.5,1.),(0.0108921325678979,0.619909717328002),
 .UNSPECIFIED.);
#143=B_SPLINE_SURFACE_WITH_KNOTS('',3,3,((#12279,#12280,#12281,#12282),
(#12283,#12284,#12285,#12286),(#12287,#12288,#12289,#12290),(#12291,#12292,
#12293,#12294),(#12295,#12296,#12297,#12298)),.UNSPECIFIED.,.F.,.F.,.F.,
(4,1,4),(4,4),(0.,0.571428571428571,1.),(0.00967450486392679,0.618764321025346),
 .UNSPECIFIED.);
#144=B_SPLINE_SURFACE_WITH_KNOTS('',3,3,((#12303,#12304,#12305,#12306),
(#12307,#12308,#12309,#12310),(#12311,#12312,#12313,#12314),(#12315,#12316,
#12317,#12318),(#12319,#12320,#12321,#12322)),.UNSPECIFIED.,.F.,.F.,.F.,
(4,1,4),(4,4),(0.,0.571428571428571,1.),(0.0097274579809394,0.618764321025346),
 .UNSPECIFIED.);
#145=B_SPLINE_SURFACE_WITH_KNOTS('',3,3,((#12327,#12328,#12329,#12330),
(#12331,#12332,#12333,#12334),(#12335,#12336,#12337,#12338),(#12339,#12340,
#12341,#12342),(#12343,#12344,#12345,#12346)),.UNSPECIFIED.,.F.,.F.,.F.,
(4,1,4),(4,4),(0.,0.571428571428571,1.),(11.3440533366984,11.6229931281671),
 .UNSPECIFIED.);
#146=B_SPLINE_SURFACE_WITH_KNOTS('',3,3,((#12347,#12348,#12349,#12350),
(#12351,#12352,#12353,#12354),(#12355,#12356,#12357,#12358),(#12359,#12360,
#12361,#12362),(#12363,#12364,#12365,#12366)),.UNSPECIFIED.,.F.,.F.,.F.,
(4,1,4),(4,4),(0.,0.5,1.),(0.0108402259132964,0.619909717328002),
 .UNSPECIFIED.);
#147=B_SPLINE_SURFACE_WITH_KNOTS('',3,3,((#12392,#12393,#12394,#12395),
(#12396,#12397,#12398,#12399),(#12400,#12401,#12402,#12403),(#12404,#12405,
#12406,#12407),(#12408,#12409,#12410,#12411)),.UNSPECIFIED.,.F.,.F.,.F.,
(4,1,4),(4,4),(0.,0.571428571428571,1.),(-0.00387706229521417,0.619909717328002),
 .UNSPECIFIED.);
#148=B_SPLINE_SURFACE_WITH_KNOTS('',3,3,((#12430,#12431,#12432,#12433,#12434,
#12435),(#12436,#12437,#12438,#12439,#12440,#12441),(#12442,#12443,#12444,
#12445,#12446,#12447),(#12448,#12449,#12450,#12451,#12452,#12453),(#12454,
#12455,#12456,#12457,#12458,#12459)),.UNSPECIFIED.,.F.,.F.,.F.,(4,1,4),
(4,1,1,4),(0.,0.571428571428571,1.),(0.270878787657975,5.14716807550265,
8.39802760073243,11.6488871259622),.UNSPECIFIED.);
#149=B_SPLINE_SURFACE_WITH_KNOTS('',3,3,((#12472,#12473,#12474,#12475),
(#12476,#12477,#12478,#12479),(#12480,#12481,#12482,#12483),(#12484,#12485,
#12486,#12487),(#12488,#12489,#12490,#12491)),.UNSPECIFIED.,.F.,.F.,.F.,
(4,1,4),(4,4),(0.,0.571428571428571,1.),(-0.00522825793187074,0.618764321025346),
 .UNSPECIFIED.);
#150=B_SPLINE_SURFACE_WITH_KNOTS('',3,3,((#12500,#12501,#12502,#12503),
(#12504,#12505,#12506,#12507),(#12508,#12509,#12510,#12511),(#12512,#12513,
#12514,#12515),(#12516,#12517,#12518,#12519)),.UNSPECIFIED.,.F.,.F.,.F.,
(4,1,4),(4,4),(0.,0.571428571428571,1.),(-0.00506942997988007,0.618764321025346),
 .UNSPECIFIED.);
#151=B_SPLINE_SURFACE_WITH_KNOTS('',3,3,((#12528,#12529,#12530,#12531,#12532),
(#12533,#12534,#12535,#12536,#12537),(#12538,#12539,#12540,#12541,#12542),
(#12543,#12544,#12545,#12546,#12547),(#12548,#12549,#12550,#12551,#12552)),
 .UNSPECIFIED.,.F.,.F.,.F.,(4,1,4),(4,1,4),(0.,0.571428571428571,1.),(0.244984789862841,
5.12127407770751,11.6229931281671),.UNSPECIFIED.);
#152=B_SPLINE_SURFACE_WITH_KNOTS('',3,3,((#12563,#12564,#12565,#12566),
(#12567,#12568,#12569,#12570),(#12571,#12572,#12573,#12574),(#12575,#12576,
#12577,#12578),(#12579,#12580,#12581,#12582)),.UNSPECIFIED.,.F.,.F.,.F.,
(4,1,4),(4,4),(0.,0.571428571428571,1.),(-0.00403278922781227,0.619909717328002),
 .UNSPECIFIED.);
#153=B_SPLINE_SURFACE_WITH_KNOTS('',3,3,((#12591,#12592,#12593,#12594),
(#12595,#12596,#12597,#12598),(#12599,#12600,#12601,#12602),(#12603,#12604,
#12605,#12606)),.UNSPECIFIED.,.F.,.F.,.F.,(4,4),(4,4),(0.0225340877622934,
0.979701609653785),(0.,0.686930956013783),.UNSPECIFIED.);
#154=B_SPLINE_SURFACE_WITH_KNOTS('',3,3,((#12609,#12610,#12611,#12612),
(#12613,#12614,#12615,#12616),(#12617,#12618,#12619,#12620),(#12621,#12622,
#12623,#12624)),.UNSPECIFIED.,.F.,.F.,.F.,(4,4),(4,4),(0.0202983903462145,
0.977465912237707),(0.,0.686930956013783),.UNSPECIFIED.);
#155=B_SPLINE_SURFACE_WITH_KNOTS('',3,3,((#12695,#12696,#12697,#12698,#12699),
(#12700,#12701,#12702,#12703,#12704),(#12705,#12706,#12707,#12708,#12709),
(#12710,#12711,#12712,#12713,#12714),(#12715,#12716,#12717,#12718,#12719)),
 .UNSPECIFIED.,.F.,.F.,.F.,(4,1,4),(4,1,4),(0.,0.571428571428571,1.),(0.,
0.0439228984074713,0.102486762950766),.UNSPECIFIED.);
#156=B_SPLINE_SURFACE_WITH_KNOTS('',3,3,((#12742,#12743,#12744,#12745,#12746),
(#12747,#12748,#12749,#12750,#12751),(#12752,#12753,#12754,#12755,#12756),
(#12757,#12758,#12759,#12760,#12761),(#12762,#12763,#12764,#12765,#12766)),
 .UNSPECIFIED.,.F.,.F.,.F.,(4,1,4),(4,1,4),(0.,0.571428571428571,1.),(0.,
0.0439228984484775,0.102486763046448),.UNSPECIFIED.);
#157=B_SPLINE_SURFACE_WITH_KNOTS('',3,3,((#12780,#12781,#12782,#12783,#12784,
#12785),(#12786,#12787,#12788,#12789,#12790,#12791),(#12792,#12793,#12794,
#12795,#12796,#12797),(#12798,#12799,#12800,#12801,#12802,#12803),(#12804,
#12805,#12806,#12807,#12808,#12809)),.UNSPECIFIED.,.F.,.F.,.F.,(4,1,4),
(4,1,1,4),(0.,0.571428571428571,1.),(0.,4.74079765360458,7.9013294226743,
11.061861191744),.UNSPECIFIED.);
#158=B_SPLINE_SURFACE_WITH_KNOTS('',3,3,((#12825,#12826,#12827,#12828,#12829),
(#12830,#12831,#12832,#12833,#12834),(#12835,#12836,#12837,#12838,#12839),
(#12840,#12841,#12842,#12843,#12844),(#12845,#12846,#12847,#12848,#12849)),
 .UNSPECIFIED.,.F.,.F.,.F.,(4,1,4),(4,1,4),(0.,0.571428571428571,1.),(0.,
0.0409389169025732,0.0955241394393374),.UNSPECIFIED.);
#159=B_SPLINE_SURFACE_WITH_KNOTS('',3,3,((#12869,#12870,#12871,#12872,#12873),
(#12874,#12875,#12876,#12877,#12878),(#12879,#12880,#12881,#12882,#12883),
(#12884,#12885,#12886,#12887,#12888),(#12889,#12890,#12891,#12892,#12893)),
 .UNSPECIFIED.,.F.,.F.,.F.,(4,1,4),(4,1,4),(0.,0.571428571428571,1.),(2.31010434703409E-17,
0.054585222365383,0.0955241391394202),.UNSPECIFIED.);
#160=B_SPLINE_SURFACE_WITH_KNOTS('',3,3,((#12907,#12908,#12909,#12910,#12911,
#12912),(#12913,#12914,#12915,#12916,#12917,#12918),(#12919,#12920,#12921,
#12922,#12923,#12924),(#12925,#12926,#12927,#12928,#12929,#12930),(#12931,
#12932,#12933,#12934,#12935,#12936)),.UNSPECIFIED.,.F.,.F.,.F.,(4,1,4),
(4,1,1,4),(0.,0.571428571428571,1.),(1.48308270761676E-15,3.16052629084276,
6.32105258168553,11.0618420179497),.UNSPECIFIED.);
#161=B_SPLINE_SURFACE_WITH_KNOTS('',3,3,((#12961,#12962,#12963,#12964),
(#12965,#12966,#12967,#12968),(#12969,#12970,#12971,#12972),(#12973,#12974,
#12975,#12976),(#12977,#12978,#12979,#12980)),.UNSPECIFIED.,.F.,.F.,.F.,
(4,1,4),(4,4),(0.,0.571428571428571,1.),(-0.0018994230917637,0.12591792480537),
 .UNSPECIFIED.);
#162=B_SPLINE_SURFACE_WITH_KNOTS('',3,3,((#13011,#13012,#13013,#13014),
(#13015,#13016,#13017,#13018),(#13019,#13020,#13021,#13022),(#13023,#13024,
#13025,#13026)),.UNSPECIFIED.,.F.,.F.,.F.,(4,4),(4,4),(0.0105624938889701,
0.988135278219398),(0.,0.624639504152193),.UNSPECIFIED.);
#163=B_SPLINE_SURFACE_WITH_KNOTS('',3,3,((#13036,#13037,#13038,#13039),
(#13040,#13041,#13042,#13043),(#13044,#13045,#13046,#13047),(#13048,#13049,
#13050,#13051),(#13052,#13053,#13054,#13055)),.UNSPECIFIED.,.F.,.F.,.F.,
(4,1,4),(4,4),(0.,0.571428571428571,1.),(-0.00248141748936713,0.125282751535517),
 .UNSPECIFIED.);
#164=B_SPLINE_SURFACE_WITH_KNOTS('',3,3,((#13097,#13098,#13099,#13100),
(#13101,#13102,#13103,#13104),(#13105,#13106,#13107,#13108),(#13109,#13110,
#13111,#13112),(#13113,#13114,#13115,#13116)),.UNSPECIFIED.,.F.,.F.,.F.,
(4,1,4),(4,4),(0.,0.571428571428571,1.),(-0.00183337806924316,0.12591792480537),
 .UNSPECIFIED.);
#165=B_SPLINE_SURFACE_WITH_KNOTS('',3,3,((#13147,#13148,#13149,#13150),
(#13151,#13152,#13153,#13154),(#13155,#13156,#13157,#13158),(#13159,#13160,
#13161,#13162),(#13163,#13164,#13165,#13166)),.UNSPECIFIED.,.F.,.F.,.F.,
(4,1,4),(4,4),(0.,0.571428571428571,1.),(-0.00256306836558615,0.125282751535516),
 .UNSPECIFIED.);
#166=B_SPLINE_SURFACE_WITH_KNOTS('',3,3,((#13205,#13206,#13207,#13208),
(#13209,#13210,#13211,#13212),(#13213,#13214,#13215,#13216),(#13217,#13218,
#13219,#13220)),.UNSPECIFIED.,.F.,.F.,.F.,(4,4),(4,4),(0.0118647217806023,
0.98943750611103),(0.,0.624639504152185),.UNSPECIFIED.);
#167=B_SPLINE_SURFACE_WITH_KNOTS('',3,3,((#15603,#15604,#15605,#15606,#15607,
#15608,#15609,#15610,#15611,#15612,#15613,#15614,#15615,#15616,#15617,#15618,
#15619,#15620,#15621,#15622,#15623,#15624,#15625,#15626,#15627,#15628,#15629,
#15630,#15631,#15632,#15633,#15634,#15635,#15636,#15637,#15638,#15639,#15640,
#15641,#15642,#15643,#15644,#15645,#15646,#15647,#15648,#15649,#15650,#15651,
#15652,#15653,#15654,#15655,#15656,#15657,#15658,#15659,#15660,#15661,#15662,
#15663,#15664,#15665,#15666,#15667,#15668,#15669,#15670,#15671,#15672,#15673,
#15674,#15675,#15676,#15677,#15678,#15679,#15680,#15681,#15682,#15683,#15684,
#15685,#15686,#15687,#15688,#15689,#15690,#15691,#15692,#15693,#15694,#15695,
#15696,#15697,#15698,#15699,#15700,#15701,#15702,#15703,#15704,#15705,#15706,
#15707,#15708,#15709,#15710,#15711,#15712,#15713,#15714,#15715,#15716,#15717,
#15718,#15719,#15720,#15721,#15722,#15723,#15724,#15725,#15726,#15727,#15728,
#15729,#15730,#15731,#15732,#15733,#15734,#15735,#15736,#15737,#15738,#15739,
#15740,#15741,#15742,#15743,#15744,#15745,#15746,#15747,#15748,#15749,#15750,
#15751,#15752,#15753,#15754,#15755,#15756,#15757,#15758,#15759,#15760,#15761,
#15762,#15763,#15764,#15765,#15766,#15767,#15768,#15769,#15770,#15771,#15772,
#15773,#15774,#15775,#15776,#15777,#15778,#15779,#15780,#15781,#15782,#15783,
#15784,#15785,#15786,#15787,#15788,#15789,#15790,#15791,#15792,#15793,#15794,
#15795,#15796,#15797,#15798),(#15799,#15800,#15801,#15802,#15803,#15804,
#15805,#15806,#15807,#15808,#15809,#15810,#15811,#15812,#15813,#15814,#15815,
#15816,#15817,#15818,#15819,#15820,#15821,#15822,#15823,#15824,#15825,#15826,
#15827,#15828,#15829,#15830,#15831,#15832,#15833,#15834,#15835,#15836,#15837,
#15838,#15839,#15840,#15841,#15842,#15843,#15844,#15845,#15846,#15847,#15848,
#15849,#15850,#15851,#15852,#15853,#15854,#15855,#15856,#15857,#15858,#15859,
#15860,#15861,#15862,#15863,#15864,#15865,#15866,#15867,#15868,#15869,#15870,
#15871,#15872,#15873,#15874,#15875,#15876,#15877,#15878,#15879,#15880,#15881,
#15882,#15883,#15884,#15885,#15886,#15887,#15888,#15889,#15890,#15891,#15892,
#15893,#15894,#15895,#15896,#15897,#15898,#15899,#15900,#15901,#15902,#15903,
#15904,#15905,#15906,#15907,#15908,#15909,#15910,#15911,#15912,#15913,#15914,
#15915,#15916,#15917,#15918,#15919,#15920,#15921,#15922,#15923,#15924,#15925,
#15926,#15927,#15928,#15929,#15930,#15931,#15932,#15933,#15934,#15935,#15936,
#15937,#15938,#15939,#15940,#15941,#15942,#15943,#15944,#15945,#15946,#15947,
#15948,#15949,#15950,#15951,#15952,#15953,#15954,#15955,#15956,#15957,#15958,
#15959,#15960,#15961,#15962,#15963,#15964,#15965,#15966,#15967,#15968,#15969,
#15970,#15971,#15972,#15973,#15974,#15975,#15976,#15977,#15978,#15979,#15980,
#15981,#15982,#15983,#15984,#15985,#15986,#15987,#15988,#15989,#15990,#15991,
#15992,#15993,#15994),(#15995,#15996,#15997,#15998,#15999,#16000,#16001,
#16002,#16003,#16004,#16005,#16006,#16007,#16008,#16009,#16010,#16011,#16012,
#16013,#16014,#16015,#16016,#16017,#16018,#16019,#16020,#16021,#16022,#16023,
#16024,#16025,#16026,#16027,#16028,#16029,#16030,#16031,#16032,#16033,#16034,
#16035,#16036,#16037,#16038,#16039,#16040,#16041,#16042,#16043,#16044,#16045,
#16046,#16047,#16048,#16049,#16050,#16051,#16052,#16053,#16054,#16055,#16056,
#16057,#16058,#16059,#16060,#16061,#16062,#16063,#16064,#16065,#16066,#16067,
#16068,#16069,#16070,#16071,#16072,#16073,#16074,#16075,#16076,#16077,#16078,
#16079,#16080,#16081,#16082,#16083,#16084,#16085,#16086,#16087,#16088,#16089,
#16090,#16091,#16092,#16093,#16094,#16095,#16096,#16097,#16098,#16099,#16100,
#16101,#16102,#16103,#16104,#16105,#16106,#16107,#16108,#16109,#16110,#16111,
#16112,#16113,#16114,#16115,#16116,#16117,#16118,#16119,#16120,#16121,#16122,
#16123,#16124,#16125,#16126,#16127,#16128,#16129,#16130,#16131,#16132,#16133,
#16134,#16135,#16136,#16137,#16138,#16139,#16140,#16141,#16142,#16143,#16144,
#16145,#16146,#16147,#16148,#16149,#16150,#16151,#16152,#16153,#16154,#16155,
#16156,#16157,#16158,#16159,#16160,#16161,#16162,#16163,#16164,#16165,#16166,
#16167,#16168,#16169,#16170,#16171,#16172,#16173,#16174,#16175,#16176,#16177,
#16178,#16179,#16180,#16181,#16182,#16183,#16184,#16185,#16186,#16187,#16188,
#16189,#16190),(#16191,#16192,#16193,#16194,#16195,#16196,#16197,#16198,
#16199,#16200,#16201,#16202,#16203,#16204,#16205,#16206,#16207,#16208,#16209,
#16210,#16211,#16212,#16213,#16214,#16215,#16216,#16217,#16218,#16219,#16220,
#16221,#16222,#16223,#16224,#16225,#16226,#16227,#16228,#16229,#16230,#16231,
#16232,#16233,#16234,#16235,#16236,#16237,#16238,#16239,#16240,#16241,#16242,
#16243,#16244,#16245,#16246,#16247,#16248,#16249,#16250,#16251,#16252,#16253,
#16254,#16255,#16256,#16257,#16258,#16259,#16260,#16261,#16262,#16263,#16264,
#16265,#16266,#16267,#16268,#16269,#16270,#16271,#16272,#16273,#16274,#16275,
#16276,#16277,#16278,#16279,#16280,#16281,#16282,#16283,#16284,#16285,#16286,
#16287,#16288,#16289,#16290,#16291,#16292,#16293,#16294,#16295,#16296,#16297,
#16298,#16299,#16300,#16301,#16302,#16303,#16304,#16305,#16306,#16307,#16308,
#16309,#16310,#16311,#16312,#16313,#16314,#16315,#16316,#16317,#16318,#16319,
#16320,#16321,#16322,#16323,#16324,#16325,#16326,#16327,#16328,#16329,#16330,
#16331,#16332,#16333,#16334,#16335,#16336,#16337,#16338,#16339,#16340,#16341,
#16342,#16343,#16344,#16345,#16346,#16347,#16348,#16349,#16350,#16351,#16352,
#16353,#16354,#16355,#16356,#16357,#16358,#16359,#16360,#16361,#16362,#16363,
#16364,#16365,#16366,#16367,#16368,#16369,#16370,#16371,#16372,#16373,#16374,
#16375,#16376,#16377,#16378,#16379,#16380,#16381,#16382,#16383,#16384,#16385,
#16386)),.UNSPECIFIED.,.F.,.F.,.F.,(4,4),(4,1,1,1,1,1,1,1,1,1,1,1,1,1,1,
1,1,1,1,1,1,1,1,1,1,1,1,1,1,1,1,1,1,1,1,1,1,1,1,1,1,1,1,1,1,1,1,1,1,1,1,
1,1,1,1,1,1,1,1,1,1,1,1,1,1,1,1,1,1,1,1,1,1,1,1,1,1,1,1,1,1,1,1,1,1,1,1,
1,1,1,1,1,1,1,1,1,1,1,1,1,1,1,1,1,1,1,1,1,1,1,1,1,1,1,1,1,1,1,1,1,1,1,1,
1,1,1,1,1,1,1,1,1,1,1,1,1,1,1,1,1,1,1,1,1,1,1,1,1,1,1,1,1,1,1,1,1,1,1,1,
1,1,1,1,1,1,1,1,1,1,1,1,1,1,1,1,1,1,1,1,1,1,1,1,1,1,1,1,1,1,1,1,1,1,4),
(0.,0.0329955678841871),(11.6159397475006,12.61358260836,13.6112254692194,
14.6088683300789,15.6065111909383,16.6041540517977,17.6017969126571,18.5994397735165,
19.5970826343759,20.5947254952353,21.5923683560947,22.5900112169541,23.5876540778135,
24.5852969386729,25.5829397995323,26.5805826603917,27.5782255212511,28.5758683821105,
29.5735112429699,30.5711541038294,31.5687969646888,32.5664398255482,33.5640826864076,
34.561725547267,35.5593684081264,36.5570112689858,37.5546541298452,38.5522969907046,
39.549939851564,40.5475827124234,41.5452255732828,42.5428684341422,43.5405112950016,
44.538154155861,45.5357970167204,46.5334398775799,47.5310827384393,48.5287255992987,
49.5263684601581,50.5240113210175,51.5216541818769,52.5192970427363,53.5169399035957,
54.5145827644551,55.5122256253145,56.5098684861739,57.5075113470333,58.5051542078927,
59.5027970687521,60.5004399296115,61.4980827904709,62.4957256513303,63.4933685121897,
64.4910113730492,65.4886542339086,66.486297094768,67.4839399556274,68.4815828164868,
69.4792256773462,70.4768685382056,71.474511399065,72.4721542599244,73.4697971207838,
74.4674399816432,75.4650828425026,76.462725703362,77.4603685642214,78.4580114250808,
79.4556542859402,80.4532971467996,81.4509400076591,82.4485828685185,83.4462257293779,
84.4438685902373,85.4415114510967,86.4391543119561,87.4367971728155,88.4344400336749,
89.4320828945343,90.4297257553937,91.4273686162531,92.4250114771125,93.4226543379719,
94.4202971988313,95.4179400596907,96.4155829205502,97.4132257814096,98.410868642269,
99.4085115031284,100.406154363988,101.403797224847,102.401440085707,103.399082946566,
104.396725807425,105.394368668285,106.392011529144,107.389654390004,108.387297250863,
109.384940111722,110.382582972582,111.380225833441,112.377868694301,113.37551155516,
114.373154416019,115.370797276879,116.368440137738,117.366082998598,118.363725859457,
119.361368720316,120.359011581176,121.356654442035,122.354297302895,123.351940163754,
124.349583024614,125.347225885473,126.344868746332,127.342511607192,128.340154468051,
129.337797328911,130.33544018977,131.333083050629,132.330725911489,133.328368772348,
134.326011633208,135.323654494067,136.321297354926,137.318940215786,138.316583076645,
139.314225937505,140.311868798364,141.309511659223,142.307154520083,143.304797380942,
144.302440241802,145.300083102661,146.29772596352,147.29536882438,148.293011685239,
149.290654546099,150.288297406958,151.285940267817,152.283583128677,153.281225989536,
154.278868850396,155.276511711255,156.274154572115,157.271797432974,158.269440293833,
159.267083154693,160.264726015552,161.262368876412,162.260011737271,163.25765459813,
164.25529745899,165.252940319849,166.250583180709,167.248226041568,168.245868902427,
169.243511763287,170.241154624146,171.238797485006,172.236440345865,173.234083206724,
174.231726067584,175.229368928443,176.227011789303,177.224654650162,178.222297511021,
179.219940371881,180.21758323274,181.2152260936,182.212868954459,183.210511815318,
184.208154676178,185.205797537037,186.203440397897,187.201083258756,188.198726119616,
189.196368980475,190.194011841334,191.191654702194,192.189297563053,193.186940423913,
194.184583284772,195.182226145631,196.179869006491,197.17751186735,198.17515472821,
199.172797589069,200.170440449928,201.168083310788,202.165726171647,203.163369032507,
204.161011893366),.UNSPECIFIED.);
#168=B_SPLINE_SURFACE_WITH_KNOTS('',3,3,((#16476,#16477,#16478,#16479,#16480,
#16481,#16482,#16483,#16484,#16485,#16486,#16487,#16488,#16489,#16490,#16491,
#16492,#16493,#16494,#16495,#16496,#16497,#16498,#16499,#16500,#16501,#16502,
#16503,#16504,#16505,#16506,#16507,#16508,#16509,#16510,#16511,#16512,#16513,
#16514,#16515,#16516,#16517,#16518,#16519,#16520,#16521,#16522,#16523,#16524,
#16525,#16526,#16527,#16528,#16529,#16530,#16531,#16532,#16533,#16534,#16535,
#16536,#16537,#16538,#16539,#16540,#16541,#16542,#16543,#16544,#16545,#16546,
#16547,#16548,#16549,#16550,#16551,#16552,#16553,#16554,#16555,#16556,#16557,
#16558,#16559,#16560,#16561,#16562,#16563,#16564,#16565,#16566,#16567,#16568,
#16569,#16570,#16571,#16572,#16573,#16574,#16575,#16576,#16577,#16578,#16579,
#16580,#16581,#16582,#16583,#16584,#16585,#16586,#16587,#16588,#16589,#16590,
#16591,#16592,#16593,#16594,#16595,#16596,#16597,#16598,#16599,#16600,#16601,
#16602,#16603,#16604,#16605,#16606,#16607,#16608,#16609,#16610,#16611,#16612,
#16613,#16614,#16615,#16616,#16617,#16618,#16619,#16620,#16621,#16622,#16623,
#16624,#16625,#16626,#16627,#16628,#16629,#16630,#16631,#16632,#16633,#16634,
#16635,#16636,#16637,#16638,#16639,#16640,#16641,#16642,#16643,#16644,#16645,
#16646,#16647,#16648,#16649,#16650,#16651,#16652,#16653,#16654,#16655,#16656,
#16657,#16658,#16659,#16660,#16661,#16662,#16663,#16664,#16665,#16666,#16667,
#16668,#16669,#16670,#16671,#16672,#16673),(#16674,#16675,#16676,#16677,
#16678,#16679,#16680,#16681,#16682,#16683,#16684,#16685,#16686,#16687,#16688,
#16689,#16690,#16691,#16692,#16693,#16694,#16695,#16696,#16697,#16698,#16699,
#16700,#16701,#16702,#16703,#16704,#16705,#16706,#16707,#16708,#16709,#16710,
#16711,#16712,#16713,#16714,#16715,#16716,#16717,#16718,#16719,#16720,#16721,
#16722,#16723,#16724,#16725,#16726,#16727,#16728,#16729,#16730,#16731,#16732,
#16733,#16734,#16735,#16736,#16737,#16738,#16739,#16740,#16741,#16742,#16743,
#16744,#16745,#16746,#16747,#16748,#16749,#16750,#16751,#16752,#16753,#16754,
#16755,#16756,#16757,#16758,#16759,#16760,#16761,#16762,#16763,#16764,#16765,
#16766,#16767,#16768,#16769,#16770,#16771,#16772,#16773,#16774,#16775,#16776,
#16777,#16778,#16779,#16780,#16781,#16782,#16783,#16784,#16785,#16786,#16787,
#16788,#16789,#16790,#16791,#16792,#16793,#16794,#16795,#16796,#16797,#16798,
#16799,#16800,#16801,#16802,#16803,#16804,#16805,#16806,#16807,#16808,#16809,
#16810,#16811,#16812,#16813,#16814,#16815,#16816,#16817,#16818,#16819,#16820,
#16821,#16822,#16823,#16824,#16825,#16826,#16827,#16828,#16829,#16830,#16831,
#16832,#16833,#16834,#16835,#16836,#16837,#16838,#16839,#16840,#16841,#16842,
#16843,#16844,#16845,#16846,#16847,#16848,#16849,#16850,#16851,#16852,#16853,
#16854,#16855,#16856,#16857,#16858,#16859,#16860,#16861,#16862,#16863,#16864,
#16865,#16866,#16867,#16868,#16869,#16870,#16871),(#16872,#16873,#16874,
#16875,#16876,#16877,#16878,#16879,#16880,#16881,#16882,#16883,#16884,#16885,
#16886,#16887,#16888,#16889,#16890,#16891,#16892,#16893,#16894,#16895,#16896,
#16897,#16898,#16899,#16900,#16901,#16902,#16903,#16904,#16905,#16906,#16907,
#16908,#16909,#16910,#16911,#16912,#16913,#16914,#16915,#16916,#16917,#16918,
#16919,#16920,#16921,#16922,#16923,#16924,#16925,#16926,#16927,#16928,#16929,
#16930,#16931,#16932,#16933,#16934,#16935,#16936,#16937,#16938,#16939,#16940,
#16941,#16942,#16943,#16944,#16945,#16946,#16947,#16948,#16949,#16950,#16951,
#16952,#16953,#16954,#16955,#16956,#16957,#16958,#16959,#16960,#16961,#16962,
#16963,#16964,#16965,#16966,#16967,#16968,#16969,#16970,#16971,#16972,#16973,
#16974,#16975,#16976,#16977,#16978,#16979,#16980,#16981,#16982,#16983,#16984,
#16985,#16986,#16987,#16988,#16989,#16990,#16991,#16992,#16993,#16994,#16995,
#16996,#16997,#16998,#16999,#17000,#17001,#17002,#17003,#17004,#17005,#17006,
#17007,#17008,#17009,#17010,#17011,#17012,#17013,#17014,#17015,#17016,#17017,
#17018,#17019,#17020,#17021,#17022,#17023,#17024,#17025,#17026,#17027,#17028,
#17029,#17030,#17031,#17032,#17033,#17034,#17035,#17036,#17037,#17038,#17039,
#17040,#17041,#17042,#17043,#17044,#17045,#17046,#17047,#17048,#17049,#17050,
#17051,#17052,#17053,#17054,#17055,#17056,#17057,#17058,#17059,#17060,#17061,
#17062,#17063,#17064,#17065,#17066,#17067,#17068,#17069),(#17070,#17071,
#17072,#17073,#17074,#17075,#17076,#17077,#17078,#17079,#17080,#17081,#17082,
#17083,#17084,#17085,#17086,#17087,#17088,#17089,#17090,#17091,#17092,#17093,
#17094,#17095,#17096,#17097,#17098,#17099,#17100,#17101,#17102,#17103,#17104,
#17105,#17106,#17107,#17108,#17109,#17110,#17111,#17112,#17113,#17114,#17115,
#17116,#17117,#17118,#17119,#17120,#17121,#17122,#17123,#17124,#17125,#17126,
#17127,#17128,#17129,#17130,#17131,#17132,#17133,#17134,#17135,#17136,#17137,
#17138,#17139,#17140,#17141,#17142,#17143,#17144,#17145,#17146,#17147,#17148,
#17149,#17150,#17151,#17152,#17153,#17154,#17155,#17156,#17157,#17158,#17159,
#17160,#17161,#17162,#17163,#17164,#17165,#17166,#17167,#17168,#17169,#17170,
#17171,#17172,#17173,#17174,#17175,#17176,#17177,#17178,#17179,#17180,#17181,
#17182,#17183,#17184,#17185,#17186,#17187,#17188,#17189,#17190,#17191,#17192,
#17193,#17194,#17195,#17196,#17197,#17198,#17199,#17200,#17201,#17202,#17203,
#17204,#17205,#17206,#17207,#17208,#17209,#17210,#17211,#17212,#17213,#17214,
#17215,#17216,#17217,#17218,#17219,#17220,#17221,#17222,#17223,#17224,#17225,
#17226,#17227,#17228,#17229,#17230,#17231,#17232,#17233,#17234,#17235,#17236,
#17237,#17238,#17239,#17240,#17241,#17242,#17243,#17244,#17245,#17246,#17247,
#17248,#17249,#17250,#17251,#17252,#17253,#17254,#17255,#17256,#17257,#17258,
#17259,#17260,#17261,#17262,#17263,#17264,#17265,#17266,#17267)),
 .UNSPECIFIED.,.F.,.F.,.F.,(4,4),(4,1,1,1,1,1,1,1,1,1,1,1,1,1,1,1,1,1,1,
1,1,1,1,1,1,1,1,1,1,1,1,1,1,1,1,1,1,1,1,1,1,1,1,1,1,1,1,1,1,1,1,1,1,1,1,
1,1,1,1,1,1,1,1,1,1,1,1,1,1,1,1,1,1,1,1,1,1,1,1,1,1,1,1,1,1,1,1,1,1,1,1,
1,1,1,1,1,1,1,1,1,1,1,1,1,1,1,1,1,1,1,1,1,1,1,1,1,1,1,1,1,1,1,1,1,1,1,1,
1,1,1,1,1,1,1,1,1,1,1,1,1,1,1,1,1,1,1,1,1,1,1,1,1,1,1,1,1,1,1,1,1,1,1,1,
1,1,1,1,1,1,1,1,1,1,1,1,1,1,1,1,1,1,1,1,1,1,1,1,1,1,1,1,1,1,1,1,4),(0.,
0.0329955678841871),(8.30203615430855,9.30007843543257,10.2981207165566,
11.2961629976806,12.2942052788047,13.2922475599287,14.2902898410527,15.2883321221767,
16.2863744033008,17.2844166844248,18.2824589655488,19.2805012466728,20.2785435277969,
21.2765858089209,22.2746280900449,23.272670371169,24.270712652293,25.268754933417,
26.266797214541,27.2648394956651,28.2628817767891,29.2609240579131,30.2589663390371,
31.2570086201612,32.2550509012852,33.2530931824092,34.2511354635333,35.2491777446573,
36.2472200257813,37.2452623069053,38.2433045880294,39.2413468691534,40.2393891502774,
41.2374314314014,42.2354737125255,43.2335159936495,44.2315582747735,45.2296005558975,
46.2276428370216,47.2256851181456,48.2237273992696,49.2217696803937,50.2198119615177,
51.2178542426417,52.2158965237657,53.2139388048898,54.2119810860138,55.2100233671378,
56.2080656482619,57.2061079293859,58.2041502105099,59.2021924916339,60.200234772758,
61.198277053882,62.196319335006,63.19436161613,64.1924038972541,65.1904461783781,
66.1884884595021,67.1865307406262,68.1845730217502,69.1826153028742,70.1806575839982,
71.1786998651223,72.1767421462463,73.1747844273703,74.1728267084943,75.1708689896184,
76.1689112707424,77.1669535518664,78.1649958329905,79.1630381141145,80.1610803952385,
81.1591226763625,82.1571649574865,83.1552072386106,84.1532495197346,85.1512918008586,
86.1493340819827,87.1473763631067,88.1454186442307,89.1434609253548,90.1415032064788,
91.1395454876028,92.1375877687268,93.1356300498508,94.1336723309749,95.1317146120989,
96.1297568932229,97.127799174347,98.125841455471,99.123883736595,100.121926017719,
101.119968298843,102.118010579967,103.116052861091,104.114095142215,105.112137423339,
106.110179704463,107.108221985587,108.106264266711,109.104306547835,110.102348828959,
111.100391110083,112.098433391207,113.096475672331,114.094517953455,115.092560234579,
116.090602515703,117.088644796828,118.086687077952,119.084729359076,120.0827716402,
121.080813921324,122.078856202448,123.076898483572,124.074940764696,125.07298304582,
126.071025326944,127.069067608068,128.067109889192,129.065152170316,130.06319445144,
131.061236732564,132.059279013688,133.057321294812,134.055363575936,135.05340585706,
136.051448138184,137.049490419308,138.047532700432,139.045574981556,140.04361726268,
141.041659543804,142.039701824928,143.037744106052,144.035786387176,145.0338286683,
146.031870949424,147.029913230548,148.027955511672,149.025997792796,150.02404007392,
151.022082355044,152.020124636168,153.018166917292,154.016209198417,155.014251479541,
156.012293760665,157.010336041789,158.008378322913,159.006420604037,160.004462885161,
161.002505166285,162.000547447409,162.998589728533,163.996632009657,164.994674290781,
165.992716571905,166.990758853029,167.988801134153,168.986843415277,169.984885696401,
170.982927977525,171.980970258649,172.979012539773,173.977054820897,174.975097102021,
175.973139383145,176.971181664269,177.969223945393,178.967266226517,179.965308507641,
180.963350788765,181.961393069889,182.959435351013,183.957477632137,184.955519913261,
185.953562194385,186.951604475509,187.949646756633,188.947689037757,189.945731318881,
190.943773600006,191.94181588113,192.939858162254,193.937900443378,194.935942724502,
195.933985005626,196.93202728675,197.930069567874,198.928111848998,199.926154130122,
200.924196411246,201.92223869237,202.920280973494),.UNSPECIFIED.);
#169=B_SPLINE_SURFACE_WITH_KNOTS('',3,3,((#17726,#17727,#17728,#17729,#17730,
#17731,#17732,#17733,#17734,#17735,#17736,#17737,#17738,#17739,#17740,#17741,
#17742,#17743,#17744,#17745,#17746,#17747,#17748,#17749,#17750,#17751,#17752,
#17753,#17754,#17755,#17756,#17757,#17758,#17759,#17760,#17761),(#17762,
#17763,#17764,#17765,#17766,#17767,#17768,#17769,#17770,#17771,#17772,#17773,
#17774,#17775,#17776,#17777,#17778,#17779,#17780,#17781,#17782,#17783,#17784,
#17785,#17786,#17787,#17788,#17789,#17790,#17791,#17792,#17793,#17794,#17795,
#17796,#17797),(#17798,#17799,#17800,#17801,#17802,#17803,#17804,#17805,
#17806,#17807,#17808,#17809,#17810,#17811,#17812,#17813,#17814,#17815,#17816,
#17817,#17818,#17819,#17820,#17821,#17822,#17823,#17824,#17825,#17826,#17827,
#17828,#17829,#17830,#17831,#17832,#17833),(#17834,#17835,#17836,#17837,
#17838,#17839,#17840,#17841,#17842,#17843,#17844,#17845,#17846,#17847,#17848,
#17849,#17850,#17851,#17852,#17853,#17854,#17855,#17856,#17857,#17858,#17859,
#17860,#17861,#17862,#17863,#17864,#17865,#17866,#17867,#17868,#17869)),
 .UNSPECIFIED.,.F.,.F.,.F.,(4,4),(4,1,1,1,1,1,1,1,1,1,1,1,1,1,1,1,1,1,1,
1,1,1,1,1,1,1,1,1,1,1,1,1,1,4),(0.,0.0321584099938622),(11.8553612635794,
12.830508595889,13.8056559281987,14.7808032605084,15.755950592818,16.7310979251277,
17.7062452574374,18.681392589747,19.6565399220567,20.6316872543664,21.606834586676,
22.5819819189857,23.5571292512954,24.532276583605,25.5074239159147,26.4825712482243,
27.457718580534,28.4328659128437,29.4080132451533,30.383160577463,31.3583079097727,
32.3334552420823,33.308602574392,34.2837499067017,35.2588972390113,36.234044571321,
37.2091919036307,38.1843392359403,39.15948656825,40.1346339005596,41.1097812328693,
42.084928565179,43.0600758974886,44.0352232297983),.UNSPECIFIED.);
#170=B_SPLINE_SURFACE_WITH_KNOTS('',3,3,((#17993,#17994,#17995,#17996,#17997,
#17998,#17999,#18000,#18001,#18002,#18003,#18004,#18005,#18006,#18007,#18008,
#18009,#18010,#18011,#18012,#18013,#18014,#18015,#18016,#18017,#18018,#18019,
#18020,#18021,#18022,#18023,#18024,#18025,#18026,#18027,#18028),(#18029,
#18030,#18031,#18032,#18033,#18034,#18035,#18036,#18037,#18038,#18039,#18040,
#18041,#18042,#18043,#18044,#18045,#18046,#18047,#18048,#18049,#18050,#18051,
#18052,#18053,#18054,#18055,#18056,#18057,#18058,#18059,#18060,#18061,#18062,
#18063,#18064),(#18065,#18066,#18067,#18068,#18069,#18070,#18071,#18072,
#18073,#18074,#18075,#18076,#18077,#18078,#18079,#18080,#18081,#18082,#18083,
#18084,#18085,#18086,#18087,#18088,#18089,#18090,#18091,#18092,#18093,#18094,
#18095,#18096,#18097,#18098,#18099,#18100),(#18101,#18102,#18103,#18104,
#18105,#18106,#18107,#18108,#18109,#18110,#18111,#18112,#18113,#18114,#18115,
#18116,#18117,#18118,#18119,#18120,#18121,#18122,#18123,#18124,#18125,#18126,
#18127,#18128,#18129,#18130,#18131,#18132,#18133,#18134,#18135,#18136)),
 .UNSPECIFIED.,.F.,.F.,.F.,(4,4),(4,1,1,1,1,1,1,1,1,1,1,1,1,1,1,1,1,1,1,
1,1,1,1,1,1,1,1,1,1,1,1,1,1,4),(0.,0.0321584099938622),(14.3984001269719,
15.3735474592815,16.3486947915912,17.3238421239009,18.2989894562105,19.2741367885202,
20.2492841208299,21.2244314531395,22.1995787854492,23.1747261177589,24.1498734500685,
25.1250207823782,26.1001681146879,27.0753154469975,28.0504627793072,29.0256101116168,
30.0007574439265,30.9759047762362,31.9510521085458,32.9261994408555,33.9013467731652,
34.8764941054748,35.8516414377845,36.8267887700942,37.8019361024038,38.7770834347135,
39.7522307670232,40.7273780993328,41.7025254316425,42.6776727639522,43.6528200962618,
44.6279674285715,45.6031147608811,46.5782620931908),.UNSPECIFIED.);
#171=B_SPLINE_CURVE_WITH_KNOTS('',3,(#8842,#8843,#8844,#8845,#8846,#8847),
 .UNSPECIFIED.,.F.,.F.,(4,2,4),(-0.607240122656937,-0.303691721894415,-0.000634514333697656),
 .UNSPECIFIED.);
#172=B_SPLINE_CURVE_WITH_KNOTS('',3,(#8849,#8850,#8851,#8852,#8853,#8854,
#8855,#8856,#8857,#8858,#8859,#8860,#8861,#8862,#8863,#8864,#8865,#8866,
#8867,#8868,#8869,#8870,#8871,#8872,#8873,#8874,#8875,#8876),
 .UNSPECIFIED.,.F.,.F.,(4,3,3,3,3,3,3,3,3,4),(-0.152223584381152,-0.128403685910756,
-0.115058138924018,-0.0911105876986024,-0.0779275105489685,-0.0651650823668383,
-0.0413494676927402,-0.0389105926748606,-0.0151313403168948,0.),
 .UNSPECIFIED.);
#173=B_SPLINE_CURVE_WITH_KNOTS('',3,(#8880,#8881,#8882,#8883,#8884,#8885,
#8886,#8887,#8888,#8889,#8890,#8891,#8892,#8893,#8894,#8895,#8896,#8897,
#8898,#8899,#8900,#8901,#8902,#8903,#8904,#8905,#8906,#8907),
 .UNSPECIFIED.,.F.,.F.,(4,3,3,3,3,3,3,3,3,4),(-0.152249917238265,-0.128484865669312,
-0.115494642307313,-0.0916985948709881,-0.0870953287403626,-0.0787006597758974,
-0.0547717013112817,-0.0393956522318865,-0.0155460991587222,0.),
 .UNSPECIFIED.);
#174=B_SPLINE_CURVE_WITH_KNOTS('',3,(#8908,#8909,#8910,#8911,#8912,#8913),
 .UNSPECIFIED.,.F.,.F.,(4,2,4),(-0.606785315485727,-0.30369188913634,-0.000179692314978108),
 .UNSPECIFIED.);
#175=B_SPLINE_CURVE_WITH_KNOTS('',3,(#8918,#8919,#8920,#8921,#8922,#8923),
 .UNSPECIFIED.,.F.,.F.,(4,2,4),(-0.606332812995025,-0.303737653350621,-0.000161665236032726),
 .UNSPECIFIED.);
#176=B_SPLINE_CURVE_WITH_KNOTS('',3,(#8925,#8926,#8927,#8928,#8929,#8930,
#8931,#8932,#8933,#8934,#8935,#8936,#8937,#8938,#8939,#8940,#8941,#8942,
#8943,#8944,#8945,#8946,#8947,#8948,#8949,#8950,#8951,#8952),
 .UNSPECIFIED.,.F.,.F.,(4,3,3,3,3,3,3,3,3,4),(-0.152301160038588,-0.128555435257278,
-0.115184785848022,-0.0912639339035621,-0.0780773216554274,-0.065267350293706,
-0.0414723266145325,-0.0390252168402571,-0.0152374671294611,0.),
 .UNSPECIFIED.);
#177=B_SPLINE_CURVE_WITH_KNOTS('',3,(#8956,#8957,#8958,#8959,#8960,#8961,
#8962,#8963,#8964,#8965,#8966,#8967,#8968,#8969,#8970,#8971,#8972,#8973,
#8974,#8975,#8976,#8977,#8978,#8979,#8980,#8981,#8982,#8983),
 .UNSPECIFIED.,.F.,.F.,(4,3,3,3,3,3,3,3,3,4),(-0.152307894271445,-0.128535938708366,
-0.115295945509717,-0.0915234088298753,-0.0870575315710991,-0.0782740392368046,
-0.0543664511067997,-0.0391484926712317,-0.0153774171089249,0.),
 .UNSPECIFIED.);
#178=B_SPLINE_CURVE_WITH_KNOTS('',3,(#8985,#8986,#8987,#8988,#8989,#8990),
 .UNSPECIFIED.,.F.,.F.,(4,2,4),(-0.607315067615316,-0.303737782617996,-0.00114390098251854),
 .UNSPECIFIED.);
#179=B_SPLINE_CURVE_WITH_KNOTS('',3,(#8996,#8997,#8998,#8999,#9000,#9001),
 .UNSPECIFIED.,.F.,.F.,(4,2,4),(-0.606335618682527,-0.303964064424246,-0.000163142902895597),
 .UNSPECIFIED.);
#180=B_SPLINE_CURVE_WITH_KNOTS('',3,(#9003,#9004,#9005,#9006,#9007,#9008,
#9009,#9010,#9011,#9012,#9013,#9014,#9015,#9016,#9017,#9018,#9019,#9020,
#9021,#9022,#9023,#9024,#9025,#9026,#9027,#9028,#9029,#9030),
 .UNSPECIFIED.,.F.,.F.,(4,3,3,3,3,3,3,3,3,4),(-0.152324888062519,-0.128571266282871,
-0.115187819092559,-0.0912644922975459,-0.0780623053857969,-0.0652705430018984,
-0.0414736125245103,-0.0390138150290758,-0.015226502089553,0.),
 .UNSPECIFIED.);
#181=B_SPLINE_CURVE_WITH_KNOTS('',3,(#9034,#9035,#9036,#9037,#9038,#9039,
#9040,#9041,#9042,#9043,#9044,#9045,#9046,#9047,#9048,#9049,#9050,#9051,
#9052,#9053,#9054,#9055,#9056,#9057,#9058,#9059,#9060,#9061),
 .UNSPECIFIED.,.F.,.F.,(4,3,3,3,3,3,3,3,3,4),(-0.152333600285603,-0.128561769460285,
-0.115331525958272,-0.0915566852459163,-0.0870792380259527,-0.0783165909319309,
-0.0544069520497563,-0.0391732033593778,-0.0153939862842036,0.),
 .UNSPECIFIED.);
#182=B_SPLINE_CURVE_WITH_KNOTS('',3,(#9063,#9064,#9065,#9066,#9067,#9068),
 .UNSPECIFIED.,.F.,.F.,(4,2,4),(-0.607765665607205,-0.303964210965506,-0.00159316434717749),
 .UNSPECIFIED.);
#183=B_SPLINE_CURVE_WITH_KNOTS('',3,(#9074,#9075,#9076,#9077,#9078,#9079),
 .UNSPECIFIED.,.F.,.F.,(4,2,4),(-0.608113833554089,-0.304405910662044,-0.00120843896277512),
 .UNSPECIFIED.);
#184=B_SPLINE_CURVE_WITH_KNOTS('',3,(#9081,#9082,#9083,#9084,#9085,#9086,
#9087,#9088,#9089,#9090,#9091,#9092,#9093,#9094,#9095,#9096,#9097,#9098,
#9099,#9100,#9101,#9102,#9103,#9104,#9105,#9106,#9107,#9108),
 .UNSPECIFIED.,.F.,.F.,(4,3,3,3,3,3,3,3,3,4),(-0.152638346832965,-0.128647829044501,
-0.117000727359648,-0.0929750760194364,-0.0775532335837778,-0.065166230851578,
-0.0413072760700971,-0.0386249916896363,-0.0148681833632798,0.),
 .UNSPECIFIED.);
#185=B_SPLINE_CURVE_WITH_KNOTS('',3,(#9112,#9113,#9114,#9115,#9116,#9117,
#9118,#9119,#9120,#9121,#9122,#9123,#9124,#9125,#9126,#9127,#9128,#9129,
#9130,#9131,#9132,#9133,#9134,#9135,#9136,#9137,#9138,#9139),
 .UNSPECIFIED.,.F.,.F.,(4,3,3,3,3,3,3,3,3,4),(-0.152712908768378,-0.128963682254188,
-0.116304008925778,-0.092453135123643,-0.0875380734791113,-0.0797852913889514,
-0.0558105568475602,-0.0400274901149945,-0.0159798645019078,0.),
 .UNSPECIFIED.);
#186=B_SPLINE_CURVE_WITH_KNOTS('',3,(#9141,#9142,#9143,#9144,#9145,#9146),
 .UNSPECIFIED.,.F.,.F.,(4,2,4),(-0.607607610897069,-0.304406883675693,-0.000702187548907163),
 .UNSPECIFIED.);
#187=B_SPLINE_CURVE_WITH_KNOTS('',3,(#9152,#9153,#9154,#9155),
 .UNSPECIFIED.,.F.,.F.,(4,4),(0.0130288733793136,0.619909717328002),
 .UNSPECIFIED.);
#188=B_SPLINE_CURVE_WITH_KNOTS('',3,(#9159,#9160,#9161,#9162),
 .UNSPECIFIED.,.F.,.F.,(4,4),(-0.619909717328002,-0.0130288733793137),
 .UNSPECIFIED.);
#189=B_SPLINE_CURVE_WITH_KNOTS('',3,(#9165,#9166,#9167,#9168,#9169,#9170,
#9171),.UNSPECIFIED.,.F.,.F.,(4,3,4),(7.87274532319472,10.4298004347969,
10.9780233963721),.UNSPECIFIED.);
#190=B_SPLINE_CURVE_WITH_KNOTS('',3,(#9172,#9173,#9174,#9175,#9176,#9177,
#9178),.UNSPECIFIED.,.F.,.F.,(4,3,4),(0.511752108249611,2.84807862798167,
3.61537599721027),.UNSPECIFIED.);
#191=B_SPLINE_CURVE_WITH_KNOTS('',3,(#9181,#9182,#9183,#9184,#9185,#9186,
#9187),.UNSPECIFIED.,.F.,.F.,(4,3,4),(3.81523717927831,5.72635044542746,
7.61820606472736),.UNSPECIFIED.);
#192=B_SPLINE_CURVE_WITH_KNOTS('',3,(#9190,#9191,#9192,#9193),
 .UNSPECIFIED.,.F.,.F.,(4,4),(7.8195516254834,10.6519234170402),
 .UNSPECIFIED.);
#193=B_SPLINE_CURVE_WITH_KNOTS('',3,(#9197,#9198,#9199,#9200),
 .UNSPECIFIED.,.F.,.F.,(4,4),(10.8550709503701,11.4839159448819),
 .UNSPECIFIED.);
#194=B_SPLINE_CURVE_WITH_KNOTS('',3,(#9201,#9202,#9203,#9204,#9205,#9206,
#9207,#9208,#9209,#9210,#9211,#9212,#9213,#9214,#9215,#9216,#9217,#9218,
#9219,#9220,#9221,#9222,#9223,#9224,#9225,#9226,#9227,#9228),
 .UNSPECIFIED.,.F.,.F.,(4,3,3,3,3,3,3,3,3,4),(0.,0.023800266251022,0.0390470051780055,
0.062864594207143,0.0692752090304052,0.0780196763370091,0.101808338076191,
0.108235461704482,0.131970324379069,0.138468980573541),.UNSPECIFIED.);
#195=B_SPLINE_CURVE_WITH_KNOTS('',3,(#9232,#9233,#9234,#9235,#9236,#9237,
#9238,#9239,#9240,#9241,#9242,#9243,#9244,#9245,#9246,#9247,#9248,#9249,
#9250,#9251,#9252,#9253,#9254,#9255,#9256,#9257,#9258,#9259,#9260,#9261,
#9262),.UNSPECIFIED.,.F.,.F.,(4,3,3,3,3,3,3,3,3,3,4),(0.,0.0536158767337707,
0.107707970980176,0.117140678528723,0.171373940961503,0.178118425384842,
0.234058785038521,0.2884659822146,0.324708667187819,0.378759781373182,0.415412568437851),
 .UNSPECIFIED.);
#196=B_SPLINE_CURVE_WITH_KNOTS('',3,(#9264,#9265,#9266,#9267),
 .UNSPECIFIED.,.F.,.F.,(4,4),(0.0202983903462145,0.977465912237707),
 .UNSPECIFIED.);
#197=B_SPLINE_CURVE_WITH_KNOTS('',3,(#9269,#9270,#9271,#9272,#9273,#9274,
#9275,#9276,#9277,#9278,#9279,#9280,#9281,#9282,#9283,#9284,#9285,#9286,
#9287,#9288,#9289,#9290,#9291,#9292,#9293,#9294,#9295,#9296,#9297,#9298,
#9299),.UNSPECIFIED.,.F.,.F.,(4,3,3,3,3,3,3,3,3,3,4),(0.,0.053547205187505,
0.107728964525782,0.117299670245694,0.171524652009909,0.189842726242433,
0.234296321023441,0.288773621215207,0.338477936388461,0.392564001789548,
0.442713223041249),.UNSPECIFIED.);
#198=B_SPLINE_CURVE_WITH_KNOTS('',3,(#9303,#9304,#9305,#9306,#9307,#9308,
#9309,#9310,#9311,#9312,#9313,#9314,#9315,#9316,#9317,#9318,#9319,#9320,
#9321,#9322,#9323,#9324,#9325,#9326,#9327,#9328,#9329,#9330,#9331,#9332,
#9333),.UNSPECIFIED.,.F.,.F.,(4,3,3,3,3,3,3,3,3,3,4),(0.,0.0535312152416108,
0.107707123412492,0.117215931328448,0.171445047002381,0.189808362521926,
0.234165405003858,0.288639615809812,0.338404447092272,0.392504428396833,
0.442708851597914),.UNSPECIFIED.);
#199=B_SPLINE_CURVE_WITH_KNOTS('',3,(#9335,#9336,#9337,#9338),
 .UNSPECIFIED.,.F.,.F.,(4,4),(0.0225340877622936,0.979701609653785),
 .UNSPECIFIED.);
#200=B_SPLINE_CURVE_WITH_KNOTS('',3,(#9340,#9341,#9342,#9343,#9344,#9345,
#9346,#9347,#9348,#9349,#9350,#9351,#9352,#9353,#9354,#9355,#9356,#9357,
#9358,#9359,#9360,#9361,#9362,#9363,#9364,#9365,#9366,#9367,#9368,#9369,
#9370),.UNSPECIFIED.,.F.,.F.,(4,3,3,3,3,3,3,3,3,3,4),(0.,0.0536458552170769,
0.107744721567334,0.117297895480617,0.171522683869793,0.178177673384308,
0.23429412186666,0.288702228477357,0.324838815929715,0.378862861687027,
0.415420074045746),.UNSPECIFIED.);
#201=B_SPLINE_CURVE_WITH_KNOTS('',3,(#9373,#9374,#9375,#9376,#9377,#9378,
#9379,#9380,#9381,#9382,#9383,#9384,#9385,#9386,#9387,#9388,#9389,#9390,
#9391,#9392,#9393,#9394,#9395,#9396,#9397,#9398,#9399,#9400),
 .UNSPECIFIED.,.F.,.F.,(4,3,3,3,3,3,3,3,3,4),(0.,0.0238098951475563,0.0390995920428052,
0.0629117710415135,0.0692953339558167,0.0780985718814299,0.101889748471939,
0.108278926258091,0.132003149848588,0.138471484390145),.UNSPECIFIED.);
#202=B_SPLINE_CURVE_WITH_KNOTS('',3,(#9402,#9403,#9404,#9405),
 .UNSPECIFIED.,.F.,.F.,(4,4),(2.05597917304345E-5,0.629200412657851),
 .UNSPECIFIED.);
#203=B_SPLINE_CURVE_WITH_KNOTS('',3,(#9408,#9409,#9410,#9411),
 .UNSPECIFIED.,.F.,.F.,(4,4),(0.832456091119126,3.6663340257767),
 .UNSPECIFIED.);
#204=B_SPLINE_CURVE_WITH_KNOTS('',3,(#9414,#9415,#9416,#9417,#9418,#9419,
#9420),.UNSPECIFIED.,.F.,.F.,(4,3,4),(3.86778652923942,5.76006783397632,
7.67277763234621),.UNSPECIFIED.);
#205=B_SPLINE_CURVE_WITH_KNOTS('',3,(#9424,#9425,#9426,#9427),
 .UNSPECIFIED.,.F.,.F.,(4,4),(11.1789026308149,11.490024089745),
 .UNSPECIFIED.);
#206=B_SPLINE_CURVE_WITH_KNOTS('',3,(#9429,#9430,#9431,#9432,#9433,#9434,
#9435,#9436,#9437,#9438,#9439,#9440,#9441,#9442,#9443,#9444,#9445,#9446,
#9447,#9448,#9449,#9450,#9451,#9452,#9453),.UNSPECIFIED.,.F.,.F.,(4,3,3,
3,3,3,3,3,4),(0.,0.0238050540413609,0.0390723036702896,0.0632692088215501,
0.0780555758269344,0.101951849921082,0.112801451778717,0.136536488207902,
0.147568670144067),.UNSPECIFIED.);
#207=B_SPLINE_CURVE_WITH_KNOTS('',3,(#9457,#9458,#9459,#9460,#9461,#9462,
#9463,#9464,#9465,#9466,#9467,#9468,#9469,#9470,#9471,#9472,#9473,#9474,
#9475,#9476,#9477,#9478,#9479,#9480,#9481),.UNSPECIFIED.,.F.,.F.,(4,3,3,
3,3,3,3,3,4),(0.,0.0238098889950854,0.0391003179068551,0.0632803937136523,
0.0780994777107358,0.101997157448698,0.112825962756833,0.136555142506291,
0.147570127973408),.UNSPECIFIED.);
#208=B_SPLINE_CURVE_WITH_KNOTS('',3,(#9483,#9484,#9485,#9486),
 .UNSPECIFIED.,.F.,.F.,(4,4),(2.41556456535008E-5,0.310979882704647),
 .UNSPECIFIED.);
#209=B_SPLINE_CURVE_WITH_KNOTS('',3,(#9498,#9499,#9500,#9501,#9502,#9503),
 .UNSPECIFIED.,.F.,.F.,(4,2,4),(-0.606744425054929,-0.30369469419025,-0.000104868936493974),
 .UNSPECIFIED.);
#210=B_SPLINE_CURVE_WITH_KNOTS('',3,(#9505,#9506,#9507,#9508,#9509,#9510),
 .UNSPECIFIED.,.F.,.F.,(4,2,4),(-0.60732337425873,-0.303694522808999,-0.000683832228057069),
 .UNSPECIFIED.);
#211=B_SPLINE_CURVE_WITH_KNOTS('',3,(#9512,#9513,#9514,#9515,#9516,#9517,
#9518,#9519,#9520,#9521,#9522,#9523,#9524,#9525,#9526,#9527,#9528,#9529,
#9530,#9531,#9532,#9533,#9534,#9535,#9536,#9537,#9538,#9539),
 .UNSPECIFIED.,.F.,.F.,(4,3,3,3,3,3,3,3,3,4),(-0.152213081758773,-0.128388856548194,
-0.115047734630008,-0.0910986092737131,-0.0779187269986961,-0.0651565114518209,
-0.0413397067626705,-0.0389038209724845,-0.0151251319644201,0.),
 .UNSPECIFIED.);
#212=B_SPLINE_CURVE_WITH_KNOTS('',3,(#9542,#9543,#9544,#9545,#9546,#9547,
#9548,#9549,#9550,#9551,#9552,#9553,#9554,#9555,#9556,#9557,#9558,#9559,
#9560,#9561,#9562,#9563,#9564,#9565,#9566,#9567,#9568,#9569),
 .UNSPECIFIED.,.F.,.F.,(4,3,3,3,3,3,3,3,3,4),(-0.152240567100014,-0.128476012965191,
-0.115503482174674,-0.0917060839439778,-0.0870941983819305,-0.0787260045726768,
-0.0547958477503903,-0.0394103419198022,-0.0155561788900784,0.),
 .UNSPECIFIED.);
#213=B_SPLINE_CURVE_WITH_KNOTS('',3,(#9586,#9587,#9588,#9589),
 .UNSPECIFIED.,.F.,.F.,(4,4),(-3.85438678954986,-0.750511952447855),
 .UNSPECIFIED.);
#214=B_SPLINE_CURVE_WITH_KNOTS('',3,(#9607,#9608,#9609,#9610),
 .UNSPECIFIED.,.F.,.F.,(4,4),(-0.54981857912664,-0.270878787657975),
 .UNSPECIFIED.);
#215=B_SPLINE_CURVE_WITH_KNOTS('',3,(#9611,#9612,#9613,#9614),
 .UNSPECIFIED.,.F.,.F.,(4,4),(-0.618764321025346,-0.0114172178585034),
 .UNSPECIFIED.);
#216=B_SPLINE_CURVE_WITH_KNOTS('',3,(#9635,#9636,#9637,#9638),
 .UNSPECIFIED.,.F.,.F.,(4,4),(0.74118252158834,3.84969085360113),
 .UNSPECIFIED.);
#217=B_SPLINE_CURVE_WITH_KNOTS('',3,(#9660,#9661,#9662,#9663),
 .UNSPECIFIED.,.F.,.F.,(4,4),(0.270878787657975,0.540284107299618),
 .UNSPECIFIED.);
#218=B_SPLINE_CURVE_WITH_KNOTS('',3,(#9666,#9667,#9668,#9669),
 .UNSPECIFIED.,.F.,.F.,(4,4),(8.04418106222393,11.1526893942367),
 .UNSPECIFIED.);
#219=B_SPLINE_CURVE_WITH_KNOTS('',3,(#9672,#9673,#9674,#9675),
 .UNSPECIFIED.,.F.,.F.,(4,4),(11.3535878085254,11.6229931281671),
 .UNSPECIFIED.);
#220=B_SPLINE_CURVE_WITH_KNOTS('',3,(#9697,#9698,#9699,#9700),
 .UNSPECIFIED.,.F.,.F.,(4,4),(-11.1433599633772,-8.03948512627517),
 .UNSPECIFIED.);
#221=B_SPLINE_CURVE_WITH_KNOTS('',3,(#9734,#9735,#9736,#9737),
 .UNSPECIFIED.,.F.,.F.,(4,4),(0.0114172178585033,0.618764321025346),
 .UNSPECIFIED.);
#222=B_SPLINE_CURVE_WITH_KNOTS('',3,(#9738,#9739,#9740,#9741),
 .UNSPECIFIED.,.F.,.F.,(4,4),(-11.6229931281671,-11.3440533366984),
 .UNSPECIFIED.);
#223=B_SPLINE_CURVE_WITH_KNOTS('',3,(#9744,#9745,#9746,#9747,#9748,#9749),
 .UNSPECIFIED.,.F.,.F.,(4,2,4),(-0.606286853269513,-0.303735636734938,-0.000134370544016882),
 .UNSPECIFIED.);
#224=B_SPLINE_CURVE_WITH_KNOTS('',3,(#9751,#9752,#9753,#9754,#9755,#9756,
#9757,#9758,#9759,#9760,#9761,#9762,#9763,#9764,#9765,#9766,#9767,#9768,
#9769,#9770,#9771,#9772,#9773,#9774,#9775,#9776,#9777,#9778),
 .UNSPECIFIED.,.F.,.F.,(4,3,3,3,3,3,3,3,3,4),(-0.152301724526365,-0.128559761662057,
-0.115189905045126,-0.0912708316251271,-0.0780855696141105,-0.0652713768517459,
-0.0414777101816728,-0.0390314967756457,-0.015242903619151,0.),
 .UNSPECIFIED.);
#225=B_SPLINE_CURVE_WITH_KNOTS('',3,(#9782,#9783,#9784,#9785,#9786,#9787,
#9788,#9789,#9790,#9791,#9792,#9793,#9794,#9795,#9796,#9797,#9798,#9799,
#9800,#9801,#9802,#9803,#9804,#9805,#9806,#9807,#9808,#9809),
 .UNSPECIFIED.,.F.,.F.,(4,3,3,3,3,3,3,3,3,4),(-0.1523073815286,-0.1285346644938,
-0.115283264026726,-0.0915123087981378,-0.0870533687950649,-0.0782507800682277,
-0.0543447803816484,-0.0391350231834537,-0.0153679399182895,0.),
 .UNSPECIFIED.);
#226=B_SPLINE_CURVE_WITH_KNOTS('',3,(#9810,#9811,#9812,#9813,#9814,#9815),
 .UNSPECIFIED.,.F.,.F.,(4,2,4),(-0.607338074051965,-0.303735662161239,-0.00118557149519966),
 .UNSPECIFIED.);
#227=B_SPLINE_CURVE_WITH_KNOTS('',3,(#9832,#9833,#9834,#9835),
 .UNSPECIFIED.,.F.,.F.,(4,4),(-7.8460657686783,-4.05419673417835),
 .UNSPECIFIED.);
#228=B_SPLINE_CURVE_WITH_KNOTS('',3,(#9856,#9857,#9858,#9859),
 .UNSPECIFIED.,.F.,.F.,(4,4),(4.04989375377528,7.85140214144331),
 .UNSPECIFIED.);
#229=B_SPLINE_CURVE_WITH_KNOTS('',3,(#9861,#9862,#9863,#9864),
 .UNSPECIFIED.,.F.,.F.,(4,4),(4.0424697743818,7.84397816204974),
 .UNSPECIFIED.);
#230=B_SPLINE_CURVE_WITH_KNOTS('',3,(#9885,#9886,#9887,#9888),
 .UNSPECIFIED.,.F.,.F.,(4,4),(-7.83967518164668,-4.0478061471468),
 .UNSPECIFIED.);
#231=B_SPLINE_CURVE_WITH_KNOTS('',3,(#9907,#9908,#9909,#9910,#9911,#9912),
 .UNSPECIFIED.,.F.,.F.,(4,2,4),(-0.606398914035431,-0.303967092551845,-0.000200694235479137),
 .UNSPECIFIED.);
#232=B_SPLINE_CURVE_WITH_KNOTS('',3,(#9914,#9915,#9916,#9917,#9918,#9919,
#9920,#9921,#9922,#9923,#9924,#9925,#9926,#9927,#9928,#9929,#9930,#9931,
#9932,#9933,#9934,#9935,#9936,#9937,#9938,#9939,#9940,#9941),
 .UNSPECIFIED.,.F.,.F.,(4,3,3,3,3,3,3,3,3,4),(-0.15233244131821,-0.128569871170003,
-0.115181988990177,-0.0912564475476021,-0.0780459432968613,-0.0652662335163151,
-0.0414674738832469,-0.0390013640446512,-0.0152139229936509,0.),
 .UNSPECIFIED.);
#233=B_SPLINE_CURVE_WITH_KNOTS('',3,(#9945,#9946,#9947,#9948,#9949,#9950,
#9951,#9952,#9953,#9954,#9955,#9956,#9957,#9958,#9959,#9960,#9961,#9962,
#9963,#9964,#9965,#9966,#9967,#9968,#9969,#9970,#9971,#9972),
 .UNSPECIFIED.,.F.,.F.,(4,3,3,3,3,3,3,3,3,4),(-0.152343297533924,-0.128571042154168,
-0.115361098257144,-0.0915841820623439,-0.0870924557961151,-0.0783628838319633,
-0.0544516462338148,-0.0392000432438046,-0.0154115240971992,0.),
 .UNSPECIFIED.);
#234=B_SPLINE_CURVE_WITH_KNOTS('',3,(#9973,#9974,#9975,#9976,#9977,#9978),
 .UNSPECIFIED.,.F.,.F.,(4,2,4),(-0.607734321217702,-0.303967174049374,-0.00153607519677973),
 .UNSPECIFIED.);
#235=B_SPLINE_CURVE_WITH_KNOTS('',3,(#9995,#9996,#9997,#9998),
 .UNSPECIFIED.,.F.,.F.,(4,4),(-10.8531956503852,-8.0457708503995),
 .UNSPECIFIED.);
#236=B_SPLINE_CURVE_WITH_KNOTS('',3,(#10019,#10020,#10021,#10022),
 .UNSPECIFIED.,.F.,.F.,(4,4),(8.05172912332209,10.8690635835914),
 .UNSPECIFIED.);
#237=B_SPLINE_CURVE_WITH_KNOTS('',3,(#10024,#10025,#10026,#10027),
 .UNSPECIFIED.,.F.,.F.,(4,4),(1.02480833223363,3.84214279250303),
 .UNSPECIFIED.);
#238=B_SPLINE_CURVE_WITH_KNOTS('',3,(#10048,#10049,#10050,#10051),
 .UNSPECIFIED.,.F.,.F.,(4,4),(-3.8481010654256,-1.04067626543981),
 .UNSPECIFIED.);
#239=B_SPLINE_CURVE_WITH_KNOTS('',3,(#10070,#10071,#10072,#10073,#10074,
#10075),.UNSPECIFIED.,.F.,.F.,(4,2,4),(-0.608301643694891,-0.304416323412316,
-0.0013178649037765),.UNSPECIFIED.);
#240=B_SPLINE_CURVE_WITH_KNOTS('',3,(#10077,#10078,#10079,#10080,#10081,
#10082,#10083,#10084,#10085,#10086,#10087,#10088,#10089,#10090,#10091,#10092,
#10093,#10094,#10095,#10096,#10097,#10098,#10099,#10100,#10101,#10102,#10103,
#10104),.UNSPECIFIED.,.F.,.F.,(4,3,3,3,3,3,3,3,3,4),(-0.152679905805259,
-0.128657903528546,-0.116982385578132,-0.0929502017086943,-0.0774957796939621,
-0.0651567901405441,-0.0412920018136918,-0.0385809476656748,-0.0148252868187304,
0.),.UNSPECIFIED.);
#241=B_SPLINE_CURVE_WITH_KNOTS('',3,(#10108,#10109,#10110,#10111,#10112,
#10113,#10114,#10115,#10116,#10117,#10118,#10119,#10120,#10121,#10122,#10123,
#10124,#10125,#10126,#10127,#10128,#10129,#10130,#10131,#10132,#10133,#10134,
#10135),.UNSPECIFIED.,.F.,.F.,(4,3,3,3,3,3,3,3,3,4),(-0.152762160496458,
-0.129013039804674,-0.116418683706179,-0.0925605502531877,-0.0875939536119484,
-0.0799546107253736,-0.055976748465099,-0.0401263304884301,-0.0160466564276224,
0.),.UNSPECIFIED.);
#242=B_SPLINE_CURVE_WITH_KNOTS('',3,(#10136,#10137,#10138,#10139,#10140,
#10141),.UNSPECIFIED.,.F.,.F.,(4,2,4),(-0.607519387555057,-0.304417308507995,
-0.000535579674449116),.UNSPECIFIED.);
#243=B_SPLINE_CURVE_WITH_KNOTS('',3,(#10159,#10160,#10161,#10162),
 .UNSPECIFIED.,.F.,.F.,(4,4),(0.012184405392802,0.619909717328002),
 .UNSPECIFIED.);
#244=B_SPLINE_CURVE_WITH_KNOTS('',3,(#10163,#10164,#10165,#10166),
 .UNSPECIFIED.,.F.,.F.,(4,4),(-11.6488871259622,-11.0550486447215),
 .UNSPECIFIED.);
#245=B_SPLINE_CURVE_WITH_KNOTS('',3,(#10189,#10190,#10191,#10192),
 .UNSPECIFIED.,.F.,.F.,(4,4),(11.0717103908866,11.6488871259622),
 .UNSPECIFIED.);
#246=B_SPLINE_CURVE_WITH_KNOTS('',3,(#10196,#10197,#10198,#10199),
 .UNSPECIFIED.,.F.,.F.,(4,4),(0.244984789862841,0.822161524938444),
 .UNSPECIFIED.);
#247=B_SPLINE_CURVE_WITH_KNOTS('',3,(#10217,#10218,#10219,#10220),
 .UNSPECIFIED.,.F.,.F.,(4,4),(-0.838823271103535,-0.244984789862841),
 .UNSPECIFIED.);
#248=B_SPLINE_CURVE_WITH_KNOTS('',3,(#10221,#10222,#10223,#10224),
 .UNSPECIFIED.,.F.,.F.,(4,4),(-0.619909717328002,-0.0121844053928019),
 .UNSPECIFIED.);
#249=B_SPLINE_CURVE_WITH_KNOTS('',3,(#10304,#10305,#10306,#10307),
 .UNSPECIFIED.,.F.,.F.,(4,4),(0.011877999214525,0.618764321025346),
 .UNSPECIFIED.);
#250=B_SPLINE_CURVE_WITH_KNOTS('',3,(#10328,#10329,#10330,#10331),
 .UNSPECIFIED.,.F.,.F.,(4,4),(-0.618764321025346,-0.0118779992145249),
 .UNSPECIFIED.);
#251=B_SPLINE_CURVE_WITH_KNOTS('',3,(#10417,#10418,#10419,#10420),
 .UNSPECIFIED.,.F.,.F.,(4,4),(-1.34441069388203E-17,0.619909717328002),
 .UNSPECIFIED.);
#252=B_SPLINE_CURVE_WITH_KNOTS('',3,(#10421,#10422,#10423,#10424),
 .UNSPECIFIED.,.F.,.F.,(4,4),(-0.619909717328002,-0.00253319281730041),
 .UNSPECIFIED.);
#253=B_SPLINE_CURVE_WITH_KNOTS('',3,(#10465,#10466,#10467,#10468,#10469,
#10470),.UNSPECIFIED.,.F.,.F.,(4,1,1,4),(-11.6488871259622,-8.39802760073243,
-5.14716807550265,-0.270878787657975),.UNSPECIFIED.);
#254=B_SPLINE_CURVE_WITH_KNOTS('',3,(#10471,#10472,#10473,#10474,#10475,
#10476),.UNSPECIFIED.,.F.,.F.,(4,1,1,4),(0.270878787657975,5.14716807550265,
8.39802760073243,11.6488871259622),.UNSPECIFIED.);
#255=B_SPLINE_CURVE_WITH_KNOTS('',3,(#10497,#10498,#10499,#10500),
 .UNSPECIFIED.,.F.,.F.,(4,4),(0.0013822243147816,0.618764321025346),
 .UNSPECIFIED.);
#256=B_SPLINE_CURVE_WITH_KNOTS('',3,(#10501,#10502,#10503,#10504),
 .UNSPECIFIED.,.F.,.F.,(4,4),(-0.618764321025346,8.06646416329215E-17),
 .UNSPECIFIED.);
#257=B_SPLINE_CURVE_WITH_KNOTS('',3,(#10525,#10526,#10527,#10528),
 .UNSPECIFIED.,.F.,.F.,(4,4),(-9.36750677027476E-17,0.618764321025346),
 .UNSPECIFIED.);
#258=B_SPLINE_CURVE_WITH_KNOTS('',3,(#10529,#10530,#10531,#10532),
 .UNSPECIFIED.,.F.,.F.,(4,4),(-0.618764321025346,-0.00138222431478148),
 .UNSPECIFIED.);
#259=B_SPLINE_CURVE_WITH_KNOTS('',3,(#10558,#10559,#10560,#10561,#10562),
 .UNSPECIFIED.,.F.,.F.,(4,1,4),(-11.6229931281671,-5.12127407770751,-0.244984789862841),
 .UNSPECIFIED.);
#260=B_SPLINE_CURVE_WITH_KNOTS('',3,(#10563,#10564,#10565,#10566,#10567),
 .UNSPECIFIED.,.F.,.F.,(4,1,4),(0.244984789862841,5.12127407770751,11.6229931281671),
 .UNSPECIFIED.);
#261=B_SPLINE_CURVE_WITH_KNOTS('',3,(#10588,#10589,#10590,#10591),
 .UNSPECIFIED.,.F.,.F.,(4,4),(0.00253319281730024,0.619909717328002),
 .UNSPECIFIED.);
#262=B_SPLINE_CURVE_WITH_KNOTS('',3,(#10592,#10593,#10594,#10595),
 .UNSPECIFIED.,.F.,.F.,(4,4),(-0.619909717328002,-2.51534904016637E-17),
 .UNSPECIFIED.);
#263=B_SPLINE_CURVE_WITH_KNOTS('',3,(#10837,#10838,#10839,#10840,#10841,
#10842),.UNSPECIFIED.,.F.,.F.,(4,2,4),(-0.607240122656937,-0.303691721894415,
-0.000634514333697656),.UNSPECIFIED.);
#264=B_SPLINE_CURVE_WITH_KNOTS('',3,(#10844,#10845,#10846,#10847,#10848,
#10849,#10850,#10851,#10852,#10853,#10854,#10855,#10856,#10857,#10858,#10859,
#10860,#10861,#10862,#10863,#10864,#10865,#10866,#10867,#10868,#10869,#10870,
#10871),.UNSPECIFIED.,.F.,.F.,(4,3,3,3,3,3,3,3,3,4),(-0.152223584381152,
-0.128403685910756,-0.115058138924018,-0.0911105876986024,-0.0779275105489685,
-0.0651650823668383,-0.0413494676927402,-0.0389105926748606,-0.0151313403168948,
0.),.UNSPECIFIED.);
#265=B_SPLINE_CURVE_WITH_KNOTS('',3,(#10875,#10876,#10877,#10878,#10879,
#10880,#10881,#10882,#10883,#10884,#10885,#10886,#10887,#10888,#10889,#10890,
#10891,#10892,#10893,#10894,#10895,#10896,#10897,#10898,#10899,#10900,#10901,
#10902),.UNSPECIFIED.,.F.,.F.,(4,3,3,3,3,3,3,3,3,4),(-0.152249917238265,
-0.128484865669312,-0.115494642307313,-0.0916985948709881,-0.0870953287403626,
-0.0787006597758974,-0.0547717013112817,-0.0393956522318865,-0.0155460991587222,
0.),.UNSPECIFIED.);
#266=B_SPLINE_CURVE_WITH_KNOTS('',3,(#10903,#10904,#10905,#10906,#10907,
#10908),.UNSPECIFIED.,.F.,.F.,(4,2,4),(-0.606785315485727,-0.30369188913634,
-0.000179692314978108),.UNSPECIFIED.);
#267=B_SPLINE_CURVE_WITH_KNOTS('',3,(#10913,#10914,#10915,#10916,#10917,
#10918),.UNSPECIFIED.,.F.,.F.,(4,2,4),(-0.606332812995025,-0.303737653350621,
-0.000161665236032726),.UNSPECIFIED.);
#268=B_SPLINE_CURVE_WITH_KNOTS('',3,(#10920,#10921,#10922,#10923,#10924,
#10925,#10926,#10927,#10928,#10929,#10930,#10931,#10932,#10933,#10934,#10935,
#10936,#10937,#10938,#10939,#10940,#10941,#10942,#10943,#10944,#10945,#10946,
#10947),.UNSPECIFIED.,.F.,.F.,(4,3,3,3,3,3,3,3,3,4),(-0.152301160038588,
-0.128555435257278,-0.115184785848022,-0.0912639339035621,-0.0780773216554274,
-0.065267350293706,-0.0414723266145325,-0.0390252168402571,-0.0152374671294611,
0.),.UNSPECIFIED.);
#269=B_SPLINE_CURVE_WITH_KNOTS('',3,(#10951,#10952,#10953,#10954,#10955,
#10956,#10957,#10958,#10959,#10960,#10961,#10962,#10963,#10964,#10965,#10966,
#10967,#10968,#10969,#10970,#10971,#10972,#10973,#10974,#10975,#10976,#10977,
#10978),.UNSPECIFIED.,.F.,.F.,(4,3,3,3,3,3,3,3,3,4),(-0.152307894271445,
-0.128535938708366,-0.115295945509717,-0.0915234088298753,-0.0870575315710991,
-0.0782740392368046,-0.0543664511067997,-0.0391484926712317,-0.0153774171089249,
0.),.UNSPECIFIED.);
#270=B_SPLINE_CURVE_WITH_KNOTS('',3,(#10980,#10981,#10982,#10983,#10984,
#10985),.UNSPECIFIED.,.F.,.F.,(4,2,4),(-0.607315067615316,-0.303737782617996,
-0.00114390098251854),.UNSPECIFIED.);
#271=B_SPLINE_CURVE_WITH_KNOTS('',3,(#10991,#10992,#10993,#10994,#10995,
#10996),.UNSPECIFIED.,.F.,.F.,(4,2,4),(-0.606335618682527,-0.303964064424246,
-0.000163142902895597),.UNSPECIFIED.);
#272=B_SPLINE_CURVE_WITH_KNOTS('',3,(#10998,#10999,#11000,#11001,#11002,
#11003,#11004,#11005,#11006,#11007,#11008,#11009,#11010,#11011,#11012,#11013,
#11014,#11015,#11016,#11017,#11018,#11019,#11020,#11021,#11022,#11023,#11024,
#11025),.UNSPECIFIED.,.F.,.F.,(4,3,3,3,3,3,3,3,3,4),(-0.152324888062519,
-0.128571266282871,-0.115187819092559,-0.0912644922975459,-0.0780623053857969,
-0.0652705430018984,-0.0414736125245103,-0.0390138150290758,-0.015226502089553,
0.),.UNSPECIFIED.);
#273=B_SPLINE_CURVE_WITH_KNOTS('',3,(#11029,#11030,#11031,#11032,#11033,
#11034,#11035,#11036,#11037,#11038,#11039,#11040,#11041,#11042,#11043,#11044,
#11045,#11046,#11047,#11048,#11049,#11050,#11051,#11052,#11053,#11054,#11055,
#11056),.UNSPECIFIED.,.F.,.F.,(4,3,3,3,3,3,3,3,3,4),(-0.152333600285603,
-0.128561769460285,-0.115331525958272,-0.0915566852459163,-0.0870792380259527,
-0.0783165909319309,-0.0544069520497563,-0.0391732033593778,-0.0153939862842036,
0.),.UNSPECIFIED.);
#274=B_SPLINE_CURVE_WITH_KNOTS('',3,(#11058,#11059,#11060,#11061,#11062,
#11063),.UNSPECIFIED.,.F.,.F.,(4,2,4),(-0.607765665607205,-0.303964210965506,
-0.00159316434717749),.UNSPECIFIED.);
#275=B_SPLINE_CURVE_WITH_KNOTS('',3,(#11069,#11070,#11071,#11072,#11073,
#11074),.UNSPECIFIED.,.F.,.F.,(4,2,4),(-0.608113833554089,-0.304405910662044,
-0.00120843896277512),.UNSPECIFIED.);
#276=B_SPLINE_CURVE_WITH_KNOTS('',3,(#11076,#11077,#11078,#11079,#11080,
#11081,#11082,#11083,#11084,#11085,#11086,#11087,#11088,#11089,#11090,#11091,
#11092,#11093,#11094,#11095,#11096,#11097,#11098,#11099,#11100,#11101,#11102,
#11103),.UNSPECIFIED.,.F.,.F.,(4,3,3,3,3,3,3,3,3,4),(-0.152638346832965,
-0.128647829044501,-0.117000727359648,-0.0929750760194364,-0.0775532335837778,
-0.065166230851578,-0.0413072760700971,-0.0386249916896363,-0.0148681833632798,
0.),.UNSPECIFIED.);
#277=B_SPLINE_CURVE_WITH_KNOTS('',3,(#11107,#11108,#11109,#11110,#11111,
#11112,#11113,#11114,#11115,#11116,#11117,#11118,#11119,#11120,#11121,#11122,
#11123,#11124,#11125,#11126,#11127,#11128,#11129,#11130,#11131,#11132,#11133,
#11134),.UNSPECIFIED.,.F.,.F.,(4,3,3,3,3,3,3,3,3,4),(-0.152712908768378,
-0.128963682254188,-0.116304008925778,-0.092453135123643,-0.0875380734791113,
-0.0797852913889514,-0.0558105568475602,-0.0400274901149945,-0.0159798645019078,
0.),.UNSPECIFIED.);
#278=B_SPLINE_CURVE_WITH_KNOTS('',3,(#11136,#11137,#11138,#11139,#11140,
#11141),.UNSPECIFIED.,.F.,.F.,(4,2,4),(-0.607607610897069,-0.304406883675693,
-0.000702187548907163),.UNSPECIFIED.);
#279=B_SPLINE_CURVE_WITH_KNOTS('',3,(#11147,#11148,#11149,#11150),
 .UNSPECIFIED.,.F.,.F.,(4,4),(0.0130288733793136,0.619909717328002),
 .UNSPECIFIED.);
#280=B_SPLINE_CURVE_WITH_KNOTS('',3,(#11154,#11155,#11156,#11157),
 .UNSPECIFIED.,.F.,.F.,(4,4),(-0.619909717328002,-0.0130288733793137),
 .UNSPECIFIED.);
#281=B_SPLINE_CURVE_WITH_KNOTS('',3,(#11160,#11161,#11162,#11163,#11164,
#11165,#11166),.UNSPECIFIED.,.F.,.F.,(4,3,4),(7.87274532319472,10.4298004347969,
10.9780233963721),.UNSPECIFIED.);
#282=B_SPLINE_CURVE_WITH_KNOTS('',3,(#11167,#11168,#11169,#11170,#11171,
#11172,#11173),.UNSPECIFIED.,.F.,.F.,(4,3,4),(0.511752108249611,2.84807862798167,
3.61537599721027),.UNSPECIFIED.);
#283=B_SPLINE_CURVE_WITH_KNOTS('',3,(#11176,#11177,#11178,#11179,#11180,
#11181,#11182),.UNSPECIFIED.,.F.,.F.,(4,3,4),(3.81523717927831,5.72635044542746,
7.61820606472736),.UNSPECIFIED.);
#284=B_SPLINE_CURVE_WITH_KNOTS('',3,(#11185,#11186,#11187,#11188),
 .UNSPECIFIED.,.F.,.F.,(4,4),(7.8195516254834,10.6519234170402),
 .UNSPECIFIED.);
#285=B_SPLINE_CURVE_WITH_KNOTS('',3,(#11192,#11193,#11194,#11195),
 .UNSPECIFIED.,.F.,.F.,(4,4),(10.8550709503701,11.4839159448819),
 .UNSPECIFIED.);
#286=B_SPLINE_CURVE_WITH_KNOTS('',3,(#11196,#11197,#11198,#11199,#11200,
#11201,#11202,#11203,#11204,#11205,#11206,#11207,#11208,#11209,#11210,#11211,
#11212,#11213,#11214,#11215,#11216,#11217,#11218,#11219,#11220,#11221,#11222,
#11223),.UNSPECIFIED.,.F.,.F.,(4,3,3,3,3,3,3,3,3,4),(0.,0.023800266251022,
0.0390470051780055,0.062864594207143,0.0692752090304052,0.0780196763370091,
0.101808338076191,0.108235461704482,0.131970324379069,0.138468980573541),
 .UNSPECIFIED.);
#287=B_SPLINE_CURVE_WITH_KNOTS('',3,(#11227,#11228,#11229,#11230,#11231,
#11232,#11233,#11234,#11235,#11236,#11237,#11238,#11239,#11240,#11241,#11242,
#11243,#11244,#11245,#11246,#11247,#11248,#11249,#11250,#11251,#11252,#11253,
#11254,#11255,#11256,#11257),.UNSPECIFIED.,.F.,.F.,(4,3,3,3,3,3,3,3,3,3,
4),(0.,0.0536158767337707,0.107707970980176,0.117140678528723,0.171373940961503,
0.178118425384842,0.234058785038521,0.2884659822146,0.324708667187819,0.378759781373182,
0.415412568437851),.UNSPECIFIED.);
#288=B_SPLINE_CURVE_WITH_KNOTS('',3,(#11259,#11260,#11261,#11262),
 .UNSPECIFIED.,.F.,.F.,(4,4),(0.0202983903462145,0.977465912237707),
 .UNSPECIFIED.);
#289=B_SPLINE_CURVE_WITH_KNOTS('',3,(#11264,#11265,#11266,#11267,#11268,
#11269,#11270,#11271,#11272,#11273,#11274,#11275,#11276,#11277,#11278,#11279,
#11280,#11281,#11282,#11283,#11284,#11285,#11286,#11287,#11288,#11289,#11290,
#11291,#11292,#11293,#11294),.UNSPECIFIED.,.F.,.F.,(4,3,3,3,3,3,3,3,3,3,
4),(0.,0.053547205187505,0.107728964525782,0.117299670245694,0.171524652009909,
0.189842726242433,0.234296321023441,0.288773621215207,0.338477936388461,
0.392564001789548,0.442713223041249),.UNSPECIFIED.);
#290=B_SPLINE_CURVE_WITH_KNOTS('',3,(#11298,#11299,#11300,#11301,#11302,
#11303,#11304,#11305,#11306,#11307,#11308,#11309,#11310,#11311,#11312,#11313,
#11314,#11315,#11316,#11317,#11318,#11319,#11320,#11321,#11322,#11323,#11324,
#11325,#11326,#11327,#11328),.UNSPECIFIED.,.F.,.F.,(4,3,3,3,3,3,3,3,3,3,
4),(0.,0.0535312152416108,0.107707123412492,0.117215931328448,0.171445047002381,
0.189808362521926,0.234165405003858,0.288639615809812,0.338404447092272,
0.392504428396833,0.442708851597914),.UNSPECIFIED.);
#291=B_SPLINE_CURVE_WITH_KNOTS('',3,(#11330,#11331,#11332,#11333),
 .UNSPECIFIED.,.F.,.F.,(4,4),(0.0225340877622936,0.979701609653785),
 .UNSPECIFIED.);
#292=B_SPLINE_CURVE_WITH_KNOTS('',3,(#11335,#11336,#11337,#11338,#11339,
#11340,#11341,#11342,#11343,#11344,#11345,#11346,#11347,#11348,#11349,#11350,
#11351,#11352,#11353,#11354,#11355,#11356,#11357,#11358,#11359,#11360,#11361,
#11362,#11363,#11364,#11365),.UNSPECIFIED.,.F.,.F.,(4,3,3,3,3,3,3,3,3,3,
4),(0.,0.0536458552170769,0.107744721567334,0.117297895480617,0.171522683869793,
0.178177673384308,0.23429412186666,0.288702228477357,0.324838815929715,
0.378862861687027,0.415420074045746),.UNSPECIFIED.);
#293=B_SPLINE_CURVE_WITH_KNOTS('',3,(#11368,#11369,#11370,#11371,#11372,
#11373,#11374,#11375,#11376,#11377,#11378,#11379,#11380,#11381,#11382,#11383,
#11384,#11385,#11386,#11387,#11388,#11389,#11390,#11391,#11392,#11393,#11394,
#11395),.UNSPECIFIED.,.F.,.F.,(4,3,3,3,3,3,3,3,3,4),(0.,0.0238098951475563,
0.0390995920428052,0.0629117710415135,0.0692953339558167,0.0780985718814299,
0.101889748471939,0.108278926258091,0.132003149848588,0.138471484390145),
 .UNSPECIFIED.);
#294=B_SPLINE_CURVE_WITH_KNOTS('',3,(#11397,#11398,#11399,#11400),
 .UNSPECIFIED.,.F.,.F.,(4,4),(2.05597917304345E-5,0.629200412657851),
 .UNSPECIFIED.);
#295=B_SPLINE_CURVE_WITH_KNOTS('',3,(#11403,#11404,#11405,#11406),
 .UNSPECIFIED.,.F.,.F.,(4,4),(0.832456091119126,3.6663340257767),
 .UNSPECIFIED.);
#296=B_SPLINE_CURVE_WITH_KNOTS('',3,(#11409,#11410,#11411,#11412,#11413,
#11414,#11415),.UNSPECIFIED.,.F.,.F.,(4,3,4),(3.86778652923942,5.76006783397632,
7.67277763234621),.UNSPECIFIED.);
#297=B_SPLINE_CURVE_WITH_KNOTS('',3,(#11419,#11420,#11421,#11422),
 .UNSPECIFIED.,.F.,.F.,(4,4),(11.1789026308149,11.490024089745),
 .UNSPECIFIED.);
#298=B_SPLINE_CURVE_WITH_KNOTS('',3,(#11424,#11425,#11426,#11427,#11428,
#11429,#11430,#11431,#11432,#11433,#11434,#11435,#11436,#11437,#11438,#11439,
#11440,#11441,#11442,#11443,#11444,#11445,#11446,#11447,#11448),
 .UNSPECIFIED.,.F.,.F.,(4,3,3,3,3,3,3,3,4),(0.,0.0238050540413609,0.0390723036702896,
0.0632692088215501,0.0780555758269344,0.101951849921082,0.112801451778717,
0.136536488207902,0.147568670144067),.UNSPECIFIED.);
#299=B_SPLINE_CURVE_WITH_KNOTS('',3,(#11452,#11453,#11454,#11455,#11456,
#11457,#11458,#11459,#11460,#11461,#11462,#11463,#11464,#11465,#11466,#11467,
#11468,#11469,#11470,#11471,#11472,#11473,#11474,#11475,#11476),
 .UNSPECIFIED.,.F.,.F.,(4,3,3,3,3,3,3,3,4),(0.,0.0238098889950854,0.0391003179068551,
0.0632803937136523,0.0780994777107358,0.101997157448698,0.112825962756833,
0.136555142506291,0.147570127973408),.UNSPECIFIED.);
#300=B_SPLINE_CURVE_WITH_KNOTS('',3,(#11478,#11479,#11480,#11481),
 .UNSPECIFIED.,.F.,.F.,(4,4),(2.41556456535008E-5,0.310979882704647),
 .UNSPECIFIED.);
#301=B_SPLINE_CURVE_WITH_KNOTS('',3,(#11493,#11494,#11495,#11496,#11497,
#11498),.UNSPECIFIED.,.F.,.F.,(4,2,4),(-0.606744425054929,-0.30369469419025,
-0.000104868936493974),.UNSPECIFIED.);
#302=B_SPLINE_CURVE_WITH_KNOTS('',3,(#11500,#11501,#11502,#11503,#11504,
#11505),.UNSPECIFIED.,.F.,.F.,(4,2,4),(-0.60732337425873,-0.303694522808999,
-0.000683832228057069),.UNSPECIFIED.);
#303=B_SPLINE_CURVE_WITH_KNOTS('',3,(#11507,#11508,#11509,#11510,#11511,
#11512,#11513,#11514,#11515,#11516,#11517,#11518,#11519,#11520,#11521,#11522,
#11523,#11524,#11525,#11526,#11527,#11528,#11529,#11530,#11531,#11532,#11533,
#11534),.UNSPECIFIED.,.F.,.F.,(4,3,3,3,3,3,3,3,3,4),(-0.152213081758773,
-0.128388856548194,-0.115047734630008,-0.0910986092737131,-0.0779187269986961,
-0.0651565114518209,-0.0413397067626705,-0.0389038209724845,-0.0151251319644201,
0.),.UNSPECIFIED.);
#304=B_SPLINE_CURVE_WITH_KNOTS('',3,(#11537,#11538,#11539,#11540,#11541,
#11542,#11543,#11544,#11545,#11546,#11547,#11548,#11549,#11550,#11551,#11552,
#11553,#11554,#11555,#11556,#11557,#11558,#11559,#11560,#11561,#11562,#11563,
#11564),.UNSPECIFIED.,.F.,.F.,(4,3,3,3,3,3,3,3,3,4),(-0.152240567100014,
-0.128476012965191,-0.115503482174674,-0.0917060839439778,-0.0870941983819305,
-0.0787260045726768,-0.0547958477503903,-0.0394103419198022,-0.0155561788900784,
0.),.UNSPECIFIED.);
#305=B_SPLINE_CURVE_WITH_KNOTS('',3,(#11581,#11582,#11583,#11584),
 .UNSPECIFIED.,.F.,.F.,(4,4),(-3.85438678954986,-0.750511952447855),
 .UNSPECIFIED.);
#306=B_SPLINE_CURVE_WITH_KNOTS('',3,(#11602,#11603,#11604,#11605),
 .UNSPECIFIED.,.F.,.F.,(4,4),(-0.54981857912664,-0.270878787657975),
 .UNSPECIFIED.);
#307=B_SPLINE_CURVE_WITH_KNOTS('',3,(#11606,#11607,#11608,#11609),
 .UNSPECIFIED.,.F.,.F.,(4,4),(-0.618764321025346,-0.0114172178585034),
 .UNSPECIFIED.);
#308=B_SPLINE_CURVE_WITH_KNOTS('',3,(#11630,#11631,#11632,#11633),
 .UNSPECIFIED.,.F.,.F.,(4,4),(0.74118252158834,3.84969085360113),
 .UNSPECIFIED.);
#309=B_SPLINE_CURVE_WITH_KNOTS('',3,(#11655,#11656,#11657,#11658),
 .UNSPECIFIED.,.F.,.F.,(4,4),(0.270878787657975,0.540284107299618),
 .UNSPECIFIED.);
#310=B_SPLINE_CURVE_WITH_KNOTS('',3,(#11661,#11662,#11663,#11664),
 .UNSPECIFIED.,.F.,.F.,(4,4),(8.04418106222393,11.1526893942367),
 .UNSPECIFIED.);
#311=B_SPLINE_CURVE_WITH_KNOTS('',3,(#11667,#11668,#11669,#11670),
 .UNSPECIFIED.,.F.,.F.,(4,4),(11.3535878085254,11.6229931281671),
 .UNSPECIFIED.);
#312=B_SPLINE_CURVE_WITH_KNOTS('',3,(#11692,#11693,#11694,#11695),
 .UNSPECIFIED.,.F.,.F.,(4,4),(-11.1433599633772,-8.03948512627517),
 .UNSPECIFIED.);
#313=B_SPLINE_CURVE_WITH_KNOTS('',3,(#11729,#11730,#11731,#11732),
 .UNSPECIFIED.,.F.,.F.,(4,4),(0.0114172178585033,0.618764321025346),
 .UNSPECIFIED.);
#314=B_SPLINE_CURVE_WITH_KNOTS('',3,(#11733,#11734,#11735,#11736),
 .UNSPECIFIED.,.F.,.F.,(4,4),(-11.6229931281671,-11.3440533366984),
 .UNSPECIFIED.);
#315=B_SPLINE_CURVE_WITH_KNOTS('',3,(#11739,#11740,#11741,#11742,#11743,
#11744),.UNSPECIFIED.,.F.,.F.,(4,2,4),(-0.606286853269513,-0.303735636734938,
-0.000134370544016882),.UNSPECIFIED.);
#316=B_SPLINE_CURVE_WITH_KNOTS('',3,(#11746,#11747,#11748,#11749,#11750,
#11751,#11752,#11753,#11754,#11755,#11756,#11757,#11758,#11759,#11760,#11761,
#11762,#11763,#11764,#11765,#11766,#11767,#11768,#11769,#11770,#11771,#11772,
#11773),.UNSPECIFIED.,.F.,.F.,(4,3,3,3,3,3,3,3,3,4),(-0.152301724526365,
-0.128559761662057,-0.115189905045126,-0.0912708316251271,-0.0780855696141105,
-0.0652713768517459,-0.0414777101816728,-0.0390314967756457,-0.015242903619151,
0.),.UNSPECIFIED.);
#317=B_SPLINE_CURVE_WITH_KNOTS('',3,(#11777,#11778,#11779,#11780,#11781,
#11782,#11783,#11784,#11785,#11786,#11787,#11788,#11789,#11790,#11791,#11792,
#11793,#11794,#11795,#11796,#11797,#11798,#11799,#11800,#11801,#11802,#11803,
#11804),.UNSPECIFIED.,.F.,.F.,(4,3,3,3,3,3,3,3,3,4),(-0.1523073815286,-0.1285346644938,
-0.115283264026726,-0.0915123087981378,-0.0870533687950649,-0.0782507800682277,
-0.0543447803816484,-0.0391350231834537,-0.0153679399182895,0.),
 .UNSPECIFIED.);
#318=B_SPLINE_CURVE_WITH_KNOTS('',3,(#11805,#11806,#11807,#11808,#11809,
#11810),.UNSPECIFIED.,.F.,.F.,(4,2,4),(-0.607338074051965,-0.303735662161239,
-0.00118557149519966),.UNSPECIFIED.);
#319=B_SPLINE_CURVE_WITH_KNOTS('',3,(#11827,#11828,#11829,#11830),
 .UNSPECIFIED.,.F.,.F.,(4,4),(-7.8460657686783,-4.05419673417835),
 .UNSPECIFIED.);
#320=B_SPLINE_CURVE_WITH_KNOTS('',3,(#11851,#11852,#11853,#11854),
 .UNSPECIFIED.,.F.,.F.,(4,4),(4.04989375377528,7.85140214144331),
 .UNSPECIFIED.);
#321=B_SPLINE_CURVE_WITH_KNOTS('',3,(#11856,#11857,#11858,#11859),
 .UNSPECIFIED.,.F.,.F.,(4,4),(4.0424697743818,7.84397816204974),
 .UNSPECIFIED.);
#322=B_SPLINE_CURVE_WITH_KNOTS('',3,(#11880,#11881,#11882,#11883),
 .UNSPECIFIED.,.F.,.F.,(4,4),(-7.83967518164668,-4.0478061471468),
 .UNSPECIFIED.);
#323=B_SPLINE_CURVE_WITH_KNOTS('',3,(#11902,#11903,#11904,#11905,#11906,
#11907),.UNSPECIFIED.,.F.,.F.,(4,2,4),(-0.606398914035431,-0.303967092551845,
-0.000200694235479137),.UNSPECIFIED.);
#324=B_SPLINE_CURVE_WITH_KNOTS('',3,(#11909,#11910,#11911,#11912,#11913,
#11914,#11915,#11916,#11917,#11918,#11919,#11920,#11921,#11922,#11923,#11924,
#11925,#11926,#11927,#11928,#11929,#11930,#11931,#11932,#11933,#11934,#11935,
#11936),.UNSPECIFIED.,.F.,.F.,(4,3,3,3,3,3,3,3,3,4),(-0.15233244131821,
-0.128569871170003,-0.115181988990177,-0.0912564475476021,-0.0780459432968613,
-0.0652662335163151,-0.0414674738832469,-0.0390013640446512,-0.0152139229936509,
0.),.UNSPECIFIED.);
#325=B_SPLINE_CURVE_WITH_KNOTS('',3,(#11940,#11941,#11942,#11943,#11944,
#11945,#11946,#11947,#11948,#11949,#11950,#11951,#11952,#11953,#11954,#11955,
#11956,#11957,#11958,#11959,#11960,#11961,#11962,#11963,#11964,#11965,#11966,
#11967),.UNSPECIFIED.,.F.,.F.,(4,3,3,3,3,3,3,3,3,4),(-0.152343297533924,
-0.128571042154168,-0.115361098257144,-0.0915841820623439,-0.0870924557961151,
-0.0783628838319633,-0.0544516462338148,-0.0392000432438046,-0.0154115240971992,
0.),.UNSPECIFIED.);
#326=B_SPLINE_CURVE_WITH_KNOTS('',3,(#11968,#11969,#11970,#11971,#11972,
#11973),.UNSPECIFIED.,.F.,.F.,(4,2,4),(-0.607734321217702,-0.303967174049374,
-0.00153607519677973),.UNSPECIFIED.);
#327=B_SPLINE_CURVE_WITH_KNOTS('',3,(#11990,#11991,#11992,#11993),
 .UNSPECIFIED.,.F.,.F.,(4,4),(-10.8531956503852,-8.0457708503995),
 .UNSPECIFIED.);
#328=B_SPLINE_CURVE_WITH_KNOTS('',3,(#12014,#12015,#12016,#12017),
 .UNSPECIFIED.,.F.,.F.,(4,4),(8.05172912332209,10.8690635835914),
 .UNSPECIFIED.);
#329=B_SPLINE_CURVE_WITH_KNOTS('',3,(#12019,#12020,#12021,#12022),
 .UNSPECIFIED.,.F.,.F.,(4,4),(1.02480833223363,3.84214279250303),
 .UNSPECIFIED.);
#330=B_SPLINE_CURVE_WITH_KNOTS('',3,(#12043,#12044,#12045,#12046),
 .UNSPECIFIED.,.F.,.F.,(4,4),(-3.8481010654256,-1.04067626543981),
 .UNSPECIFIED.);
#331=B_SPLINE_CURVE_WITH_KNOTS('',3,(#12065,#12066,#12067,#12068,#12069,
#12070),.UNSPECIFIED.,.F.,.F.,(4,2,4),(-0.608301643694891,-0.304416323412316,
-0.0013178649037765),.UNSPECIFIED.);
#332=B_SPLINE_CURVE_WITH_KNOTS('',3,(#12072,#12073,#12074,#12075,#12076,
#12077,#12078,#12079,#12080,#12081,#12082,#12083,#12084,#12085,#12086,#12087,
#12088,#12089,#12090,#12091,#12092,#12093,#12094,#12095,#12096,#12097,#12098,
#12099),.UNSPECIFIED.,.F.,.F.,(4,3,3,3,3,3,3,3,3,4),(-0.152679905805259,
-0.128657903528546,-0.116982385578132,-0.0929502017086943,-0.0774957796939621,
-0.0651567901405441,-0.0412920018136918,-0.0385809476656748,-0.0148252868187304,
0.),.UNSPECIFIED.);
#333=B_SPLINE_CURVE_WITH_KNOTS('',3,(#12103,#12104,#12105,#12106,#12107,
#12108,#12109,#12110,#12111,#12112,#12113,#12114,#12115,#12116,#12117,#12118,
#12119,#12120,#12121,#12122,#12123,#12124,#12125,#12126,#12127,#12128,#12129,
#12130),.UNSPECIFIED.,.F.,.F.,(4,3,3,3,3,3,3,3,3,4),(-0.152762160496458,
-0.129013039804674,-0.116418683706179,-0.0925605502531877,-0.0875939536119484,
-0.0799546107253736,-0.055976748465099,-0.0401263304884301,-0.0160466564276224,
0.),.UNSPECIFIED.);
#334=B_SPLINE_CURVE_WITH_KNOTS('',3,(#12131,#12132,#12133,#12134,#12135,
#12136),.UNSPECIFIED.,.F.,.F.,(4,2,4),(-0.607519387555057,-0.304417308507995,
-0.000535579674449116),.UNSPECIFIED.);
#335=B_SPLINE_CURVE_WITH_KNOTS('',3,(#12154,#12155,#12156,#12157),
 .UNSPECIFIED.,.F.,.F.,(4,4),(0.012184405392802,0.619909717328002),
 .UNSPECIFIED.);
#336=B_SPLINE_CURVE_WITH_KNOTS('',3,(#12158,#12159,#12160,#12161),
 .UNSPECIFIED.,.F.,.F.,(4,4),(-11.6488871259622,-11.0550486447215),
 .UNSPECIFIED.);
#337=B_SPLINE_CURVE_WITH_KNOTS('',3,(#12184,#12185,#12186,#12187),
 .UNSPECIFIED.,.F.,.F.,(4,4),(11.0717103908866,11.6488871259622),
 .UNSPECIFIED.);
#338=B_SPLINE_CURVE_WITH_KNOTS('',3,(#12191,#12192,#12193,#12194),
 .UNSPECIFIED.,.F.,.F.,(4,4),(0.244984789862841,0.822161524938444),
 .UNSPECIFIED.);
#339=B_SPLINE_CURVE_WITH_KNOTS('',3,(#12212,#12213,#12214,#12215),
 .UNSPECIFIED.,.F.,.F.,(4,4),(-0.838823271103535,-0.244984789862841),
 .UNSPECIFIED.);
#340=B_SPLINE_CURVE_WITH_KNOTS('',3,(#12216,#12217,#12218,#12219),
 .UNSPECIFIED.,.F.,.F.,(4,4),(-0.619909717328002,-0.0121844053928019),
 .UNSPECIFIED.);
#341=B_SPLINE_CURVE_WITH_KNOTS('',3,(#12299,#12300,#12301,#12302),
 .UNSPECIFIED.,.F.,.F.,(4,4),(0.011877999214525,0.618764321025346),
 .UNSPECIFIED.);
#342=B_SPLINE_CURVE_WITH_KNOTS('',3,(#12323,#12324,#12325,#12326),
 .UNSPECIFIED.,.F.,.F.,(4,4),(-0.618764321025346,-0.0118779992145249),
 .UNSPECIFIED.);
#343=B_SPLINE_CURVE_WITH_KNOTS('',3,(#12412,#12413,#12414,#12415),
 .UNSPECIFIED.,.F.,.F.,(4,4),(-1.34441069388203E-17,0.619909717328002),
 .UNSPECIFIED.);
#344=B_SPLINE_CURVE_WITH_KNOTS('',3,(#12416,#12417,#12418,#12419),
 .UNSPECIFIED.,.F.,.F.,(4,4),(-0.619909717328002,-0.00253319281730041),
 .UNSPECIFIED.);
#345=B_SPLINE_CURVE_WITH_KNOTS('',3,(#12460,#12461,#12462,#12463,#12464,
#12465),.UNSPECIFIED.,.F.,.F.,(4,1,1,4),(-11.6488871259622,-8.39802760073243,
-5.14716807550265,-0.270878787657975),.UNSPECIFIED.);
#346=B_SPLINE_CURVE_WITH_KNOTS('',3,(#12466,#12467,#12468,#12469,#12470,
#12471),.UNSPECIFIED.,.F.,.F.,(4,1,1,4),(0.270878787657975,5.14716807550265,
8.39802760073243,11.6488871259622),.UNSPECIFIED.);
#347=B_SPLINE_CURVE_WITH_KNOTS('',3,(#12492,#12493,#12494,#12495),
 .UNSPECIFIED.,.F.,.F.,(4,4),(0.0013822243147816,0.618764321025346),
 .UNSPECIFIED.);
#348=B_SPLINE_CURVE_WITH_KNOTS('',3,(#12496,#12497,#12498,#12499),
 .UNSPECIFIED.,.F.,.F.,(4,4),(-0.618764321025346,8.06646416329215E-17),
 .UNSPECIFIED.);
#349=B_SPLINE_CURVE_WITH_KNOTS('',3,(#12520,#12521,#12522,#12523),
 .UNSPECIFIED.,.F.,.F.,(4,4),(-9.36750677027476E-17,0.618764321025346),
 .UNSPECIFIED.);
#350=B_SPLINE_CURVE_WITH_KNOTS('',3,(#12524,#12525,#12526,#12527),
 .UNSPECIFIED.,.F.,.F.,(4,4),(-0.618764321025346,-0.00138222431478148),
 .UNSPECIFIED.);
#351=B_SPLINE_CURVE_WITH_KNOTS('',3,(#12553,#12554,#12555,#12556,#12557),
 .UNSPECIFIED.,.F.,.F.,(4,1,4),(-11.6229931281671,-5.12127407770751,-0.244984789862841),
 .UNSPECIFIED.);
#352=B_SPLINE_CURVE_WITH_KNOTS('',3,(#12558,#12559,#12560,#12561,#12562),
 .UNSPECIFIED.,.F.,.F.,(4,1,4),(0.244984789862841,5.12127407770751,11.6229931281671),
 .UNSPECIFIED.);
#353=B_SPLINE_CURVE_WITH_KNOTS('',3,(#12583,#12584,#12585,#12586),
 .UNSPECIFIED.,.F.,.F.,(4,4),(0.00253319281730024,0.619909717328002),
 .UNSPECIFIED.);
#354=B_SPLINE_CURVE_WITH_KNOTS('',3,(#12587,#12588,#12589,#12590),
 .UNSPECIFIED.,.F.,.F.,(4,4),(-0.619909717328002,-2.51534904016637E-17),
 .UNSPECIFIED.);
#355=B_SPLINE_CURVE_WITH_KNOTS('',3,(#12724,#12725,#12726,#12727,#12728),
 .UNSPECIFIED.,.F.,.F.,(4,1,4),(-0.102486762950766,-0.0439228984074713,
0.),.UNSPECIFIED.);
#356=B_SPLINE_CURVE_WITH_KNOTS('',3,(#12731,#12732,#12733,#12734,#12735),
 .UNSPECIFIED.,.F.,.F.,(4,1,4),(0.,0.0439228984074713,0.102486762950766),
 .UNSPECIFIED.);
#357=B_SPLINE_CURVE_WITH_KNOTS('',3,(#12770,#12771,#12772,#12773,#12774),
 .UNSPECIFIED.,.F.,.F.,(4,1,4),(-0.102486763046448,-0.0439228984484775,
0.),.UNSPECIFIED.);
#358=B_SPLINE_CURVE_WITH_KNOTS('',3,(#12775,#12776,#12777,#12778,#12779),
 .UNSPECIFIED.,.F.,.F.,(4,1,4),(0.,0.0439228984484775,0.102486763046448),
 .UNSPECIFIED.);
#359=B_SPLINE_CURVE_WITH_KNOTS('',3,(#12813,#12814,#12815,#12816,#12817,
#12818),.UNSPECIFIED.,.F.,.F.,(4,1,1,4),(-11.061861191744,-7.9013294226743,
-4.74079765360458,0.),.UNSPECIFIED.);
#360=B_SPLINE_CURVE_WITH_KNOTS('',3,(#12819,#12820,#12821,#12822,#12823,
#12824),.UNSPECIFIED.,.F.,.F.,(4,1,1,4),(0.,4.74079765360458,7.9013294226743,
11.061861191744),.UNSPECIFIED.);
#361=B_SPLINE_CURVE_WITH_KNOTS('',3,(#12853,#12854,#12855,#12856,#12857),
 .UNSPECIFIED.,.F.,.F.,(4,1,4),(-0.0955241394393374,-0.0409389169025732,
0.),.UNSPECIFIED.);
#362=B_SPLINE_CURVE_WITH_KNOTS('',3,(#12858,#12859,#12860,#12861,#12862),
 .UNSPECIFIED.,.F.,.F.,(4,1,4),(0.,0.0409389169025732,0.0955241394393374),
 .UNSPECIFIED.);
#363=B_SPLINE_CURVE_WITH_KNOTS('',3,(#12897,#12898,#12899,#12900,#12901),
 .UNSPECIFIED.,.F.,.F.,(4,1,4),(-0.0955241391394202,-0.054585222365383,
-2.31010434703409E-17),.UNSPECIFIED.);
#364=B_SPLINE_CURVE_WITH_KNOTS('',3,(#12902,#12903,#12904,#12905,#12906),
 .UNSPECIFIED.,.F.,.F.,(4,1,4),(2.31010434703409E-17,0.054585222365383,
0.0955241391394202),.UNSPECIFIED.);
#365=B_SPLINE_CURVE_WITH_KNOTS('',3,(#12937,#12938,#12939,#12940,#12941,
#12942),.UNSPECIFIED.,.F.,.F.,(4,1,1,4),(-11.0618420179497,-6.32105258168553,
-3.16052629084276,-1.48308270761676E-15),.UNSPECIFIED.);
#366=B_SPLINE_CURVE_WITH_KNOTS('',3,(#12943,#12944,#12945,#12946,#12947,
#12948),.UNSPECIFIED.,.F.,.F.,(4,1,1,4),(1.48308270761676E-15,3.16052629084276,
6.32105258168553,11.0618420179497),.UNSPECIFIED.);
#367=B_SPLINE_CURVE_WITH_KNOTS('',3,(#12951,#12952,#12953,#12954),
 .UNSPECIFIED.,.F.,.F.,(4,4),(0.00139191041679171,0.12591792480537),
 .UNSPECIFIED.);
#368=B_SPLINE_CURVE_WITH_KNOTS('',3,(#12957,#12958,#12959,#12960),
 .UNSPECIFIED.,.F.,.F.,(4,4),(-0.12591792480537,-0.00139191041679165),
 .UNSPECIFIED.);
#369=B_SPLINE_CURVE_WITH_KNOTS('',3,(#12982,#12983,#12984,#12985),
 .UNSPECIFIED.,.F.,.F.,(4,4),(-0.125267757839186,2.34187669256869E-17),
 .UNSPECIFIED.);
#370=B_SPLINE_CURVE_WITH_KNOTS('',3,(#12986,#12987,#12988,#12989,#12990,
#12991,#12992,#12993,#12994,#12995,#12996,#12997,#12998,#12999,#13000,#13001,
#13002,#13003,#13004,#13005,#13006,#13007,#13008,#13009,#13010),
 .UNSPECIFIED.,.F.,.F.,(4,3,3,3,3,3,3,3,4),(0.,0.0322618866145428,0.0585630993998112,
0.0880157356071287,0.11701919887454,0.14936655709923,0.161132799378038,
0.193259076308563,0.205272292311979),.UNSPECIFIED.);
#371=B_SPLINE_CURVE_WITH_KNOTS('',3,(#13028,#13029,#13030,#13031),
 .UNSPECIFIED.,.F.,.F.,(4,4),(-1.85615411929518E-16,0.12492953807382),
 .UNSPECIFIED.);
#372=B_SPLINE_CURVE_WITH_KNOTS('',3,(#13032,#13033,#13034,#13035),
 .UNSPECIFIED.,.F.,.F.,(4,4),(0.0105624938889701,0.988135278219398),
 .UNSPECIFIED.);
#373=B_SPLINE_CURVE_WITH_KNOTS('',3,(#13057,#13058,#13059,#13060),
 .UNSPECIFIED.,.F.,.F.,(4,4),(-0.125282751535517,-0.000756099764976127),
 .UNSPECIFIED.);
#374=B_SPLINE_CURVE_WITH_KNOTS('',3,(#13061,#13062,#13063,#13064,#13065,
#13066,#13067,#13068,#13069,#13070,#13071,#13072,#13073,#13074,#13075,#13076,
#13077,#13078,#13079,#13080,#13081,#13082,#13083,#13084,#13085,#13086,#13087,
#13088),.UNSPECIFIED.,.F.,.F.,(4,3,3,3,3,3,3,3,3,4),(0.,0.0322721186185131,
0.0586507621648183,0.090893271235385,0.0944607523249211,0.117149429440675,
0.149538018358679,0.168700492523839,0.200858914363656,0.220277485057336),
 .UNSPECIFIED.);
#375=B_SPLINE_CURVE_WITH_KNOTS('',3,(#13092,#13093,#13094,#13095),
 .UNSPECIFIED.,.F.,.F.,(4,4),(0.000756099764976051,0.125282751535516),
 .UNSPECIFIED.);
#376=B_SPLINE_CURVE_WITH_KNOTS('',3,(#13118,#13119,#13120,#13121,#13122,
#13123,#13124,#13125,#13126,#13127,#13128,#13129,#13130,#13131,#13132,#13133,
#13134,#13135,#13136,#13137,#13138,#13139,#13140,#13141,#13142),
 .UNSPECIFIED.,.F.,.F.,(4,3,3,3,3,3,3,3,4),(-1.38777878078145E-17,0.0322740250441291,
0.0586501551213245,0.0880475535304867,0.117148640042868,0.149495851515852,
0.161204029299056,0.193312734374797,0.205276387553207),.UNSPECIFIED.);
#377=B_SPLINE_CURVE_WITH_KNOTS('',3,(#13143,#13144,#13145,#13146),
 .UNSPECIFIED.,.F.,.F.,(4,4),(5.20417042793042E-18,0.125267757839184),
 .UNSPECIFIED.);
#378=B_SPLINE_CURVE_WITH_KNOTS('',3,(#13168,#13169,#13170,#13171),
 .UNSPECIFIED.,.F.,.F.,(4,4),(-0.124929538073804,-1.0547118733939E-15),
 .UNSPECIFIED.);
#379=B_SPLINE_CURVE_WITH_KNOTS('',3,(#13172,#13173,#13174,#13175,#13176,
#13177,#13178,#13179,#13180,#13181,#13182,#13183,#13184,#13185,#13186,#13187,
#13188,#13189,#13190,#13191,#13192,#13193,#13194,#13195,#13196,#13197,#13198,
#13199),.UNSPECIFIED.,.F.,.F.,(4,3,3,3,3,3,3,3,3,4),(0.,0.0322648940196546,
0.0586047006713273,0.0908498906869236,0.0944423330072586,0.117077542275299,
0.149464200283694,0.168660330271145,0.200827593216919,0.220275105166519),
 .UNSPECIFIED.);
#380=B_SPLINE_CURVE_WITH_KNOTS('',3,(#13201,#13202,#13203,#13204),
 .UNSPECIFIED.,.F.,.F.,(4,4),(0.0118647217806024,0.98943750611103),
 .UNSPECIFIED.);
#381=B_SPLINE_CURVE_WITH_KNOTS('',3,(#13227,#13228,#13229,#13230,#13231,
#13232,#13233,#13234,#13235,#13236),.UNSPECIFIED.,.F.,.F.,(4,3,3,4),(-4.09202352044852,
-3.99057144343763,-2.99292858257822,-2.07317267331971),.UNSPECIFIED.);
#382=B_SPLINE_CURVE_WITH_KNOTS('',3,(#13239,#13240,#13241,#13242,#13243,
#13244,#13245),.UNSPECIFIED.,.F.,.F.,(4,3,4),(0.,0.998042281124014,1.12274180646116),
 .UNSPECIFIED.);
#383=B_SPLINE_CURVE_WITH_KNOTS('',3,(#13250,#13251,#13252,#13253,#13254,
#13255,#13256,#13257,#13258,#13259,#13260,#13261,#13262,#13263,#13264,#13265,
#13266,#13267,#13268,#13269,#13270,#13271),.UNSPECIFIED.,.F.,.F.,(4,3,3,
3,3,3,3,4),(-10.3752088276281,-9.97642860859406,-8.97878574773466,-7.98114288687525,
-6.98350002601584,-5.98585716515644,-4.98821430429703,-4.09202352044852),
 .UNSPECIFIED.);
#384=B_SPLINE_CURVE_WITH_KNOTS('',3,(#13272,#13273,#13274,#13275,#13276,
#13277,#13278,#13279,#13280,#13281,#13282,#13283,#13284,#13285,#13286,#13287,
#13288,#13289,#13290,#13291,#13292,#13293),.UNSPECIFIED.,.F.,.F.,(4,3,3,
3,3,3,3,4),(1.12274180646116,1.99608456224804,2.99412684337208,3.99216912449611,
4.99021140562014,5.98825368674417,6.98629596786821,7.40592711364074),
 .UNSPECIFIED.);
#385=B_SPLINE_CURVE_WITH_KNOTS('',3,(#13298,#13299,#13300,#13301,#13302,
#13303,#13304,#13305,#13306,#13307,#13308,#13309,#13310,#13311,#13312,#13313,
#13314,#13315,#13316,#13317,#13318,#13319),.UNSPECIFIED.,.F.,.F.,(4,3,3,
3,3,3,3,4),(-16.6583941348077,-15.9622857737505,-14.9646429128911,-13.9670000520317,
-12.9693571911723,-11.9717143303129,-10.9740714694535,-10.3752088276281),
 .UNSPECIFIED.);
#386=B_SPLINE_CURVE_WITH_KNOTS('',3,(#13320,#13321,#13322,#13323,#13324,
#13325,#13326,#13327,#13328,#13329,#13330,#13331,#13332,#13333,#13334,#13335,
#13336,#13337,#13338,#13339,#13340,#13341),.UNSPECIFIED.,.F.,.F.,(4,3,3,
3,3,3,3,4),(7.40592711364074,7.98433824899223,8.98238053011626,9.98042281124028,
10.9784650923643,11.9765073734883,12.9745496546124,13.6891124208203),
 .UNSPECIFIED.);
#387=B_SPLINE_CURVE_WITH_KNOTS('',3,(#13346,#13347,#13348,#13349,#13350,
#13351,#13352,#13353,#13354,#13355,#13356,#13357,#13358,#13359,#13360,#13361,
#13362,#13363,#13364,#13365,#13366,#13367),.UNSPECIFIED.,.F.,.F.,(4,3,3,
3,3,3,3,4),(-22.9415794419873,-21.9481429389069,-20.9505000780475,-19.9528572171881,
-18.9552143563287,-17.9575714954693,-16.9599286346099,-16.6583941348077),
 .UNSPECIFIED.);
#388=B_SPLINE_CURVE_WITH_KNOTS('',3,(#13368,#13369,#13370,#13371,#13372,
#13373,#13374,#13375,#13376,#13377,#13378,#13379,#13380,#13381,#13382,#13383,
#13384,#13385,#13386,#13387,#13388,#13389,#13390,#13391,#13392),
 .UNSPECIFIED.,.F.,.F.,(4,3,3,3,3,3,3,3,4),(13.6891124208203,13.9725919357364,
14.9706342168604,15.9686764979844,16.9667187791085,17.9647610602325,18.9628033413565,
19.9608456224805,19.9722977279999),.UNSPECIFIED.);
#389=B_SPLINE_CURVE_WITH_KNOTS('',3,(#13397,#13398,#13399,#13400,#13401,
#13402,#13403,#13404,#13405,#13406,#13407,#13408,#13409,#13410,#13411,#13412,
#13413,#13414,#13415,#13416,#13417,#13418),.UNSPECIFIED.,.F.,.F.,(4,3,3,
3,3,3,3,4),(-29.2247647491669,-28.9316429649228,-27.9340001040634,-26.936357243204,
-25.9387143823446,-24.9410715214852,-23.9434286606257,-22.9415794419873),
 .UNSPECIFIED.);
#390=B_SPLINE_CURVE_WITH_KNOTS('',3,(#13419,#13420,#13421,#13422,#13423,
#13424,#13425,#13426,#13427,#13428,#13429,#13430,#13431,#13432,#13433,#13434,
#13435,#13436,#13437,#13438,#13439,#13440),.UNSPECIFIED.,.F.,.F.,(4,3,3,
3,3,3,3,4),(19.9722977279999,20.9588879036046,21.9569301847286,22.9549724658526,
23.9530147469767,24.9510570281007,25.9490993092247,26.2554830351795),
 .UNSPECIFIED.);
#391=B_SPLINE_CURVE_WITH_KNOTS('',3,(#13445,#13446,#13447,#13448,#13449,
#13450,#13451,#13452,#13453,#13454,#13455,#13456,#13457,#13458,#13459,#13460,
#13461,#13462,#13463,#13464,#13465,#13466),.UNSPECIFIED.,.F.,.F.,(4,3,3,
3,3,3,3,4),(-35.5079500563465,-34.9175001300792,-33.9198572692198,-32.9222144083604,
-31.924571547501,-30.9269286866416,-29.9292858257822,-29.2247647491669),
 .UNSPECIFIED.);
#392=B_SPLINE_CURVE_WITH_KNOTS('',3,(#13467,#13468,#13469,#13470,#13471,
#13472,#13473,#13474,#13475,#13476,#13477,#13478,#13479,#13480,#13481,#13482,
#13483,#13484,#13485,#13486,#13487,#13488),.UNSPECIFIED.,.F.,.F.,(4,3,3,
3,3,3,3,4),(26.2554830351795,26.9471415903487,27.9451838714728,28.9432261525968,
29.9412684337208,30.9393107148448,31.9373529959689,32.5386683423591),
 .UNSPECIFIED.);
#393=B_SPLINE_CURVE_WITH_KNOTS('',3,(#13493,#13494,#13495,#13496,#13497,
#13498,#13499,#13500,#13501,#13502,#13503,#13504,#13505,#13506,#13507,#13508,
#13509,#13510,#13511,#13512,#13513,#13514),.UNSPECIFIED.,.F.,.F.,(4,3,3,
3,3,3,3,4),(-41.791135363526,-40.9033572952357,-39.9057144343762,-38.9080715735168,
-37.9104287126574,-36.912785851798,-35.9151429909386,-35.5079500563465),
 .UNSPECIFIED.);
#394=B_SPLINE_CURVE_WITH_KNOTS('',3,(#13515,#13516,#13517,#13518,#13519,
#13520,#13521,#13522,#13523,#13524,#13525,#13526,#13527,#13528,#13529,#13530,
#13531,#13532,#13533,#13534,#13535,#13536),.UNSPECIFIED.,.F.,.F.,(4,3,3,
3,3,3,3,4),(32.5386683423591,32.9353952770929,33.9334375582169,34.931479839341,
35.929522120465,36.927564401589,37.9256066827131,38.8218536495387),
 .UNSPECIFIED.);
#395=B_SPLINE_CURVE_WITH_KNOTS('',3,(#13541,#13542,#13543,#13544,#13545,
#13546,#13547,#13548,#13549,#13550,#13551,#13552,#13553,#13554,#13555,#13556,
#13557,#13558,#13559,#13560,#13561,#13562,#13563,#13564,#13565),
 .UNSPECIFIED.,.F.,.F.,(4,3,3,3,3,3,3,3,4),(-48.0743206707056,-47.8868573212515,
-46.8892144603921,-45.8915715995327,-44.8939287386733,-43.8962858778139,
-42.8986430169545,-41.9010001560951,-41.791135363526),.UNSPECIFIED.);
#396=B_SPLINE_CURVE_WITH_KNOTS('',3,(#13566,#13567,#13568,#13569,#13570,
#13571,#13572,#13573,#13574,#13575,#13576,#13577,#13578,#13579,#13580,#13581,
#13582,#13583,#13584,#13585,#13586,#13587,#13588,#13589,#13590),
 .UNSPECIFIED.,.F.,.F.,(4,3,3,3,3,3,3,3,4),(38.8218536495387,38.9236489638371,
39.9216912449611,40.9197335260851,41.9177758072091,42.9158180883332,43.9138603694572,
44.9119026505812,45.1050389567183),.UNSPECIFIED.);
#397=B_SPLINE_CURVE_WITH_KNOTS('',3,(#13595,#13596,#13597,#13598,#13599,
#13600,#13601,#13602,#13603,#13604,#13605,#13606,#13607,#13608,#13609,#13610,
#13611,#13612,#13613,#13614,#13615,#13616),.UNSPECIFIED.,.F.,.F.,(4,3,3,
3,3,3,3,4),(-54.3575059778852,-53.8727144864079,-52.8750716255485,-51.8774287646891,
-50.8797859038297,-49.8821430429703,-48.8845001821109,-48.0743206707056),
 .UNSPECIFIED.);
#398=B_SPLINE_CURVE_WITH_KNOTS('',3,(#13617,#13618,#13619,#13620,#13621,
#13622,#13623,#13624,#13625,#13626,#13627,#13628,#13629,#13630,#13631,#13632,
#13633,#13634,#13635,#13636,#13637,#13638),.UNSPECIFIED.,.F.,.F.,(4,3,3,
3,3,3,3,4),(45.1050389567183,45.9099449317052,46.9079872128293,47.9060294939533,
48.9040717750773,49.9021140562014,50.9001563373254,51.3882242638979),
 .UNSPECIFIED.);
#399=B_SPLINE_CURVE_WITH_KNOTS('',3,(#13643,#13644,#13645,#13646,#13647,
#13648,#13649,#13650,#13651,#13652,#13653,#13654,#13655,#13656,#13657,#13658,
#13659,#13660,#13661,#13662,#13663,#13664),.UNSPECIFIED.,.F.,.F.,(4,3,3,
3,3,3,3,4),(-60.6406912850648,-59.8585716515644,-58.860928790705,-57.8632859298455,
-56.8656430689861,-55.8680002081267,-54.8703573472673,-54.3575059778852),
 .UNSPECIFIED.);
#400=B_SPLINE_CURVE_WITH_KNOTS('',3,(#13665,#13666,#13667,#13668,#13669,
#13670,#13671,#13672,#13673,#13674,#13675,#13676,#13677,#13678,#13679,#13680,
#13681,#13682,#13683,#13684,#13685,#13686),.UNSPECIFIED.,.F.,.F.,(4,3,3,
3,3,3,3,4),(51.3882242638979,51.8981986184494,52.8962408995734,53.8942831806975,
54.8923254618215,55.8903677429455,56.8884100240695,57.6714095710775),
 .UNSPECIFIED.);
#401=B_SPLINE_CURVE_WITH_KNOTS('',3,(#13691,#13692,#13693,#13694,#13695,
#13696,#13697,#13698,#13699,#13700,#13701,#13702,#13703,#13704,#13705,#13706,
#13707,#13708,#13709,#13710,#13711,#13712,#13713,#13714,#13715),
 .UNSPECIFIED.,.F.,.F.,(4,3,3,3,3,3,3,3,4),(-66.9238765922444,-66.8420716775802,
-65.8444288167208,-64.8467859558614,-63.849143095002,-62.8515002341426,
-61.8538573732832,-60.8562145124238,-60.6406912850648),.UNSPECIFIED.);
#402=B_SPLINE_CURVE_WITH_KNOTS('',3,(#13716,#13717,#13718,#13719,#13720,
#13721,#13722,#13723,#13724,#13725,#13726,#13727,#13728,#13729,#13730,#13731,
#13732,#13733,#13734,#13735,#13736,#13737,#13738,#13739,#13740),
 .UNSPECIFIED.,.F.,.F.,(4,3,3,3,3,3,3,3,4),(57.6714095710775,57.8864523051936,
58.8844945863176,59.8825368674416,60.8805791485657,61.8786214296897,62.8766637108137,
63.8747059919378,63.9545948782571),.UNSPECIFIED.);
#403=B_SPLINE_CURVE_WITH_KNOTS('',3,(#13745,#13746,#13747,#13748,#13749,
#13750,#13751,#13752,#13753,#13754,#13755,#13756,#13757,#13758,#13759,#13760,
#13761,#13762,#13763,#13764,#13765,#13766),.UNSPECIFIED.,.F.,.F.,(4,3,3,
3,3,3,3,4),(-73.207061899424,-72.8279288427366,-71.8302859818773,-70.8326431210178,
-69.8350002601584,-68.837357399299,-67.8397145384396,-66.9238765922444),
 .UNSPECIFIED.);
#404=B_SPLINE_CURVE_WITH_KNOTS('',3,(#13767,#13768,#13769,#13770,#13771,
#13772,#13773,#13774,#13775,#13776,#13777,#13778,#13779,#13780,#13781,#13782,
#13783,#13784,#13785,#13786,#13787,#13788),.UNSPECIFIED.,.F.,.F.,(4,3,3,
3,3,3,3,4),(63.9545948782571,64.8727482730618,65.8707905541858,66.8688328353098,
67.8668751164338,68.8649173975579,69.8629596786819,70.2377801854366),
 .UNSPECIFIED.);
#405=B_SPLINE_CURVE_WITH_KNOTS('',3,(#13793,#13794,#13795,#13796,#13797,
#13798,#13799,#13800,#13801,#13802,#13803,#13804,#13805,#13806,#13807,#13808,
#13809,#13810,#13811,#13812,#13813,#13814),.UNSPECIFIED.,.F.,.F.,(4,3,3,
3,3,3,3,4),(-79.4902472066036,-78.8137860078931,-77.8161431470337,-76.8185002861743,
-75.8208574253149,-74.8232145644555,-73.825571703596,-73.207061899424),
 .UNSPECIFIED.);
#406=B_SPLINE_CURVE_WITH_KNOTS('',3,(#13815,#13816,#13817,#13818,#13819,
#13820,#13821,#13822,#13823,#13824,#13825,#13826,#13827,#13828,#13829,#13830,
#13831,#13832,#13833,#13834,#13835,#13836),.UNSPECIFIED.,.F.,.F.,(4,3,3,
3,3,3,3,4),(70.2377801854366,70.8610019598059,71.85904424093,72.857086522054,
73.855128803178,74.853171084302,75.8512133654261,76.5209654926162),
 .UNSPECIFIED.);
#407=B_SPLINE_CURVE_WITH_KNOTS('',3,(#13841,#13842,#13843,#13844,#13845,
#13846,#13847,#13848,#13849,#13850,#13851,#13852,#13853,#13854,#13855,#13856,
#13857,#13858,#13859,#13860,#13861,#13862),.UNSPECIFIED.,.F.,.F.,(4,3,3,
3,3,3,3,4),(-85.7734325137832,-84.7996431730495,-83.8020003121901,-82.8043574513307,
-81.8067145904713,-80.8090717296119,-79.8114288687525,-79.4902472066036),
 .UNSPECIFIED.);
#408=B_SPLINE_CURVE_WITH_KNOTS('',3,(#13863,#13864,#13865,#13866,#13867,
#13868,#13869,#13870,#13871,#13872,#13873,#13874,#13875,#13876,#13877,#13878,
#13879,#13880,#13881,#13882,#13883,#13884),.UNSPECIFIED.,.F.,.F.,(4,3,3,
3,3,3,3,4),(76.5209654926162,76.8492556465501,77.8472979276741,78.8453402087982,
79.8433824899222,80.8414247710462,81.8394670521702,82.8041507997958),
 .UNSPECIFIED.);
#409=B_SPLINE_CURVE_WITH_KNOTS('',3,(#13889,#13890,#13891,#13892,#13893,
#13894,#13895,#13896,#13897,#13898,#13899,#13900,#13901,#13902,#13903,#13904,
#13905,#13906,#13907,#13908,#13909,#13910,#13911,#13912,#13913),
 .UNSPECIFIED.,.F.,.F.,(4,3,3,3,3,3,3,3,4),(-92.0566178209628,-91.7831431990654,
-90.7855003382059,-89.7878574773465,-88.7902146164871,-87.7925717556277,
-86.7949288947683,-85.7972860339089,-85.7734325137832),.UNSPECIFIED.);
#410=B_SPLINE_CURVE_WITH_KNOTS('',3,(#13914,#13915,#13916,#13917,#13918,
#13919,#13920,#13921,#13922,#13923,#13924,#13925,#13926,#13927,#13928,#13929,
#13930,#13931,#13932,#13933,#13934,#13935,#13936,#13937,#13938),
 .UNSPECIFIED.,.F.,.F.,(4,3,3,3,3,3,3,3,4),(82.8041507997958,82.8375093332942,
83.8355516144183,84.8335938955423,85.8316361766664,86.8296784577904,87.8277207389144,
88.8257630200384,89.0873361069754),.UNSPECIFIED.);
#411=B_SPLINE_CURVE_WITH_KNOTS('',3,(#13943,#13944,#13945,#13946,#13947,
#13948,#13949,#13950,#13951,#13952,#13953,#13954,#13955,#13956,#13957,#13958,
#13959,#13960,#13961,#13962,#13963,#13964),.UNSPECIFIED.,.F.,.F.,(4,3,3,
3,3,3,3,4),(-98.3398031281424,-97.7690003642218,-96.7713575033624,-95.773714642503,
-94.7760717816436,-93.7784289207842,-92.7807860599248,-92.0566178209628),
 .UNSPECIFIED.);
#412=B_SPLINE_CURVE_WITH_KNOTS('',3,(#13965,#13966,#13967,#13968,#13969,
#13970,#13971,#13972,#13973,#13974,#13975,#13976,#13977,#13978,#13979,#13980,
#13981,#13982,#13983,#13984,#13985,#13986),.UNSPECIFIED.,.F.,.F.,(4,3,3,
3,3,3,3,4),(89.0873361069754,89.8238053011624,90.8218475822865,91.8198898634105,
92.8179321445345,93.8159744256585,94.8140167067826,95.370521414155),
 .UNSPECIFIED.);
#413=B_SPLINE_CURVE_WITH_KNOTS('',3,(#13991,#13992,#13993,#13994,#13995,
#13996,#13997,#13998,#13999,#14000,#14001,#14002,#14003,#14004,#14005,#14006,
#14007,#14008,#14009,#14010,#14011,#14012),.UNSPECIFIED.,.F.,.F.,(4,3,3,
3,3,3,3,4),(-104.622988435322,-103.754857529378,-102.757214668519,-101.759571807659,
-100.7619289468,-99.7642860859406,-98.7666432250812,-98.3398031281424),
 .UNSPECIFIED.);
#414=B_SPLINE_CURVE_WITH_KNOTS('',3,(#14013,#14014,#14015,#14016,#14017,
#14018,#14019,#14020,#14021,#14022,#14023,#14024,#14025,#14026,#14027,#14028,
#14029,#14030,#14031,#14032,#14033,#14034),.UNSPECIFIED.,.F.,.F.,(4,3,3,
3,3,3,3,4),(95.370521414155,95.8120589879066,96.8101012690306,97.8081435501546,
98.8061858312787,99.8042281124027,100.802270393527,101.653706721335),
 .UNSPECIFIED.);
#415=B_SPLINE_CURVE_WITH_KNOTS('',3,(#14039,#14040,#14041,#14042,#14043,
#14044,#14045,#14046,#14047,#14048,#14049,#14050,#14051,#14052,#14053,#14054,
#14055,#14056,#14057,#14058,#14059,#14060,#14061,#14062,#14063),
 .UNSPECIFIED.,.F.,.F.,(4,3,3,3,3,3,3,3,4),(-110.906173742502,-110.738357555394,
-109.740714694535,-108.743071833675,-107.745428972816,-106.747786111956,
-105.750143251097,-104.752500390238,-104.622988435322),.UNSPECIFIED.);
#416=B_SPLINE_CURVE_WITH_KNOTS('',3,(#14064,#14065,#14066,#14067,#14068,
#14069,#14070,#14071,#14072,#14073,#14074,#14075,#14076,#14077,#14078,#14079,
#14080,#14081,#14082,#14083,#14084,#14085,#14086,#14087,#14088),
 .UNSPECIFIED.,.F.,.F.,(4,3,3,3,3,3,3,3,4),(101.653706721335,101.800312674651,
102.798354955775,103.796397236899,104.794439518023,105.792481799147,106.790524080271,
107.788566361395,107.936892028514),.UNSPECIFIED.);
#417=B_SPLINE_CURVE_WITH_KNOTS('',3,(#14093,#14094,#14095,#14096,#14097,
#14098,#14099,#14100,#14101,#14102,#14103,#14104,#14105,#14106,#14107,#14108,
#14109,#14110,#14111,#14112,#14113,#14114),.UNSPECIFIED.,.F.,.F.,(4,3,3,
3,3,3,3,4),(-117.189359049681,-116.724214720551,-115.726571859691,-114.728928998832,
-113.731286137972,-112.733643277113,-111.736000416253,-110.906173742502),
 .UNSPECIFIED.);
#418=B_SPLINE_CURVE_WITH_KNOTS('',3,(#14115,#14116,#14117,#14118,#14119,
#14120,#14121,#14122,#14123,#14124,#14125,#14126,#14127,#14128,#14129,#14130,
#14131,#14132,#14133,#14134,#14135,#14136),.UNSPECIFIED.,.F.,.F.,(4,3,3,
3,3,3,3,4),(107.936892028514,108.786608642519,109.784650923643,110.782693204767,
111.780735485891,112.778777767015,113.776820048139,114.220077335694),
 .UNSPECIFIED.);
#419=B_SPLINE_CURVE_WITH_KNOTS('',3,(#14141,#14142,#14143,#14144,#14145,
#14146,#14147,#14148,#14149,#14150,#14151,#14152,#14153,#14154,#14155,#14156,
#14157,#14158,#14159,#14160,#14161,#14162),.UNSPECIFIED.,.F.,.F.,(4,3,3,
3,3,3,3,4),(-123.472544356861,-122.710071885707,-121.712429024848,-120.714786163988,
-119.717143303129,-118.719500442269,-117.72185758141,-117.189359049681),
 .UNSPECIFIED.);
#420=B_SPLINE_CURVE_WITH_KNOTS('',3,(#14163,#14164,#14165,#14166,#14167,
#14168,#14169,#14170,#14171,#14172,#14173,#14174,#14175,#14176,#14177,#14178,
#14179,#14180,#14181,#14182,#14183,#14184),.UNSPECIFIED.,.F.,.F.,(4,3,3,
3,3,3,3,4),(114.220077335694,114.774862329263,115.772904610387,116.770946891511,
117.768989172635,118.767031453759,119.765073734883,120.503262642873),
 .UNSPECIFIED.);
#421=B_SPLINE_CURVE_WITH_KNOTS('',3,(#14189,#14190,#14191,#14192,#14193,
#14194,#14195,#14196,#14197,#14198,#14199,#14200,#14201,#14202,#14203,#14204,
#14205,#14206,#14207,#14208,#14209,#14210,#14211,#14212,#14213),
 .UNSPECIFIED.,.F.,.F.,(4,3,3,3,3,3,3,3,4),(-129.75572966404,-129.693571911723,
-128.695929050863,-127.698286190004,-126.700643329145,-125.703000468285,
-124.705357607426,-123.707714746566,-123.472544356861),.UNSPECIFIED.);
#422=B_SPLINE_CURVE_WITH_KNOTS('',3,(#14214,#14215,#14216,#14217,#14218,
#14219,#14220,#14221,#14222,#14223,#14224,#14225,#14226,#14227,#14228,#14229,
#14230,#14231,#14232,#14233,#14234,#14235,#14236,#14237,#14238),
 .UNSPECIFIED.,.F.,.F.,(4,3,3,3,3,3,3,3,4),(120.503262642873,120.763116016007,
121.761158297131,122.759200578255,123.757242859379,124.755285140503,125.753327421627,
126.751369702751,126.786447950053),.UNSPECIFIED.);
#423=B_SPLINE_CURVE_WITH_KNOTS('',3,(#14243,#14244,#14245,#14246,#14247,
#14248,#14249,#14250,#14251,#14252,#14253,#14254,#14255,#14256,#14257,#14258,
#14259,#14260,#14261,#14262,#14263,#14264),.UNSPECIFIED.,.F.,.F.,(4,3,3,
3,3,3,3,4),(-136.03891497122,-135.679429076879,-134.68178621602,-133.68414335516,
-132.686500494301,-131.688857633442,-130.691214772582,-129.75572966404),
 .UNSPECIFIED.);
#424=B_SPLINE_CURVE_WITH_KNOTS('',3,(#14265,#14266,#14267,#14268,#14269,
#14270,#14271,#14272,#14273,#14274,#14275,#14276,#14277,#14278,#14279,#14280,
#14281,#14282,#14283,#14284,#14285,#14286),.UNSPECIFIED.,.F.,.F.,(4,3,3,
3,3,3,3,4),(126.786447950053,127.749411983875,128.747454265,129.745496546124,
130.743538827248,131.741581108372,132.739623389496,133.069633257233),
 .UNSPECIFIED.);
#425=B_SPLINE_CURVE_WITH_KNOTS('',3,(#14291,#14292,#14293,#14294,#14295,
#14296,#14297,#14298,#14299,#14300,#14301,#14302,#14303,#14304,#14305,#14306,
#14307,#14308,#14309,#14310,#14311,#14312),.UNSPECIFIED.,.F.,.F.,(4,3,3,
3,3,3,3,4),(-142.322100278399,-141.665286242036,-140.667643381176,-139.670000520317,
-138.672357659457,-137.674714798598,-136.677071937739,-136.03891497122),
 .UNSPECIFIED.);
#426=B_SPLINE_CURVE_WITH_KNOTS('',3,(#14313,#14314,#14315,#14316,#14317,
#14318,#14319,#14320,#14321,#14322,#14323,#14324,#14325,#14326,#14327,#14328,
#14329,#14330,#14331,#14332,#14333,#14334),.UNSPECIFIED.,.F.,.F.,(4,3,3,
3,3,3,3,4),(133.069633257233,133.73766567062,134.735707951744,135.733750232868,
136.731792513992,137.729834795116,138.72787707624,139.352818564412),
 .UNSPECIFIED.);
#427=B_SPLINE_CURVE_WITH_KNOTS('',3,(#14339,#14340,#14341,#14342,#14343,
#14344,#14345,#14346,#14347,#14348,#14349,#14350,#14351,#14352,#14353,#14354,
#14355,#14356,#14357,#14358,#14359,#14360),.UNSPECIFIED.,.F.,.F.,(4,3,3,
3,3,3,3,4),(-148.605285585579,-147.651143407192,-146.653500546333,-145.655857685473,
-144.658214824614,-143.660571963754,-142.662929102895,-142.322100278399),
 .UNSPECIFIED.);
#428=B_SPLINE_CURVE_WITH_KNOTS('',3,(#14361,#14362,#14363,#14364,#14365,
#14366,#14367,#14368,#14369,#14370,#14371,#14372,#14373,#14374,#14375,#14376,
#14377,#14378,#14379,#14380,#14381,#14382),.UNSPECIFIED.,.F.,.F.,(4,3,3,
3,3,3,3,4),(139.352818564412,139.725919357364,140.723961638488,141.722003919612,
142.720046200736,143.71808848186,144.716130762984,145.636003871592),
 .UNSPECIFIED.);
#429=B_SPLINE_CURVE_WITH_KNOTS('',3,(#14387,#14388,#14389,#14390,#14391,
#14392,#14393,#14394,#14395,#14396,#14397,#14398,#14399,#14400,#14401,#14402,
#14403,#14404,#14405,#14406,#14407,#14408,#14409,#14410,#14411),
 .UNSPECIFIED.,.F.,.F.,(4,3,3,3,3,3,3,3,4),(-154.888470892759,-154.634643433208,
-153.637000572349,-152.639357711489,-151.64171485063,-150.64407198977,-149.646429128911,
-148.648786268052,-148.605285585579),.UNSPECIFIED.);
#430=B_SPLINE_CURVE_WITH_KNOTS('',3,(#14412,#14413,#14414,#14415,#14416,
#14417,#14418,#14419,#14420,#14421,#14422,#14423,#14424,#14425,#14426,#14427,
#14428,#14429,#14430,#14431,#14432,#14433,#14434,#14435,#14436),
 .UNSPECIFIED.,.F.,.F.,(4,3,3,3,3,3,3,3,4),(145.636003871592,145.714173044108,
146.712215325232,147.710257606356,148.70829988748,149.706342168604,150.704384449728,
151.702426730852,151.919189178771),.UNSPECIFIED.);
#431=B_SPLINE_CURVE_WITH_KNOTS('',3,(#14441,#14442,#14443,#14444,#14445,
#14446,#14447,#14448,#14449,#14450,#14451,#14452,#14453,#14454,#14455,#14456,
#14457,#14458,#14459,#14460,#14461,#14462),.UNSPECIFIED.,.F.,.F.,(4,3,3,
3,3,3,3,4),(-161.171656199938,-160.620500598364,-159.622857737505,-158.625214876646,
-157.627572015786,-156.629929154927,-155.632286294067,-154.888470892759),
 .UNSPECIFIED.);
#432=B_SPLINE_CURVE_WITH_KNOTS('',3,(#14463,#14464,#14465,#14466,#14467,
#14468,#14469,#14470,#14471,#14472,#14473,#14474,#14475,#14476,#14477,#14478,
#14479,#14480,#14481,#14482,#14483,#14484),.UNSPECIFIED.,.F.,.F.,(4,3,3,
3,3,3,3,4),(151.919189178771,152.700469011976,153.6985112931,154.696553574224,
155.694595855348,156.692638136472,157.690680417596,158.202374485951),
 .UNSPECIFIED.);
#433=B_SPLINE_CURVE_WITH_KNOTS('',3,(#14489,#14490,#14491,#14492,#14493,
#14494,#14495,#14496,#14497,#14498,#14499,#14500,#14501,#14502,#14503,#14504,
#14505,#14506,#14507,#14508,#14509,#14510),.UNSPECIFIED.,.F.,.F.,(4,3,3,
3,3,3,3,4),(-167.454841507118,-166.606357763521,-165.608714902661,-164.611072041802,
-163.613429180943,-162.615786320083,-161.618143459224,-161.171656199938),
 .UNSPECIFIED.);
#434=B_SPLINE_CURVE_WITH_KNOTS('',3,(#14511,#14512,#14513,#14514,#14515,
#14516,#14517,#14518,#14519,#14520,#14521,#14522,#14523,#14524,#14525,#14526,
#14527,#14528,#14529,#14530,#14531,#14532),.UNSPECIFIED.,.F.,.F.,(4,3,3,
3,3,3,3,4),(158.202374485951,158.68872269872,159.686764979844,160.684807260968,
161.682849542092,162.680891823216,163.67893410434,164.48555979313),
 .UNSPECIFIED.);
#435=B_SPLINE_CURVE_WITH_KNOTS('',3,(#14537,#14538,#14539,#14540,#14541,
#14542,#14543,#14544,#14545,#14546,#14547,#14548,#14549,#14550,#14551,#14552,
#14553,#14554,#14555,#14556,#14557,#14558,#14559,#14560,#14561),
 .UNSPECIFIED.,.F.,.F.,(4,3,3,3,3,3,3,3,4),(-173.738026814297,-173.589857789537,
-172.592214928677,-171.594572067818,-170.596929206958,-169.599286346099,
-168.60164348524,-167.60400062438,-167.454841507118),.UNSPECIFIED.);
#436=B_SPLINE_CURVE_WITH_KNOTS('',3,(#14562,#14563,#14564,#14565,#14566,
#14567,#14568,#14569,#14570,#14571,#14572,#14573,#14574,#14575,#14576,#14577,
#14578,#14579,#14580,#14581,#14582,#14583,#14584,#14585,#14586),
 .UNSPECIFIED.,.F.,.F.,(4,3,3,3,3,3,3,3,4),(164.48555979313,164.676976385465,
165.675018666588,166.673060947713,167.671103228837,168.669145509961,169.667187791085,
170.665230072209,170.76874510031),.UNSPECIFIED.);
#437=B_SPLINE_CURVE_WITH_KNOTS('',3,(#14591,#14592,#14593,#14594,#14595,
#14596,#14597,#14598,#14599,#14600,#14601,#14602,#14603,#14604,#14605,#14606,
#14607,#14608,#14609,#14610,#14611,#14612),.UNSPECIFIED.,.F.,.F.,(4,3,3,
3,3,3,3,4),(-180.021212121477,-179.575714954693,-178.578072093834,-177.580429232974,
-176.582786372115,-175.585143511255,-174.587500650396,-173.738026814297),
 .UNSPECIFIED.);
#438=B_SPLINE_CURVE_WITH_KNOTS('',3,(#14613,#14614,#14615,#14616,#14617,
#14618,#14619,#14620,#14621,#14622,#14623,#14624,#14625,#14626,#14627,#14628,
#14629,#14630,#14631,#14632,#14633,#14634),.UNSPECIFIED.,.F.,.F.,(4,3,3,
3,3,3,3,4),(170.76874510031,171.663272353333,172.661314634457,173.659356915581,
174.657399196705,175.655441477829,176.653483758953,177.051930407489),
 .UNSPECIFIED.);
#439=B_SPLINE_CURVE_WITH_KNOTS('',3,(#14639,#14640,#14641,#14642,#14643,
#14644,#14645,#14646,#14647,#14648,#14649,#14650,#14651,#14652,#14653,#14654,
#14655,#14656,#14657,#14658,#14659,#14660),.UNSPECIFIED.,.F.,.F.,(4,3,3,
3,3,3,3,4),(-186.304397428656,-185.56157211985,-184.56392925899,-183.566286398131,
-182.568643537271,-181.571000676412,-180.573357815553,-180.021212121477),
 .UNSPECIFIED.);
#440=B_SPLINE_CURVE_WITH_KNOTS('',3,(#14661,#14662,#14663,#14664,#14665,
#14666,#14667,#14668,#14669,#14670,#14671,#14672,#14673,#14674,#14675,#14676,
#14677,#14678,#14679,#14680,#14681,#14682),.UNSPECIFIED.,.F.,.F.,(4,3,3,
3,3,3,3,4),(177.051930407489,177.651526040077,178.649568321201,179.647610602325,
180.645652883449,181.643695164573,182.641737445697,183.335115714669),
 .UNSPECIFIED.);
#441=B_SPLINE_CURVE_WITH_KNOTS('',3,(#14688,#14689,#14690,#14691,#14692,
#14693,#14694,#14695,#14696,#14697),.UNSPECIFIED.,.F.,.F.,(4,1,1,1,1,1,
1,4),(197.920337176157,198.17515472821,199.172797589069,200.170440449928,
201.168083310788,202.165726171647,203.163369032507,204.161011893366),
 .UNSPECIFIED.);
#442=B_SPLINE_CURVE_WITH_KNOTS('',3,(#14700,#14701,#14702,#14703,#14704,
#14705,#14706,#14707,#14708),.UNSPECIFIED.,.F.,.F.,(4,1,1,1,1,1,4),(197.920337176157,
197.930069567874,198.928111848998,199.926154130122,200.924196411246,201.92223869237,
202.920280973494),.UNSPECIFIED.);
#443=B_SPLINE_CURVE_WITH_KNOTS('',3,(#14713,#14714,#14715,#14716,#14717,
#14718,#14719,#14720,#14721,#14722),.UNSPECIFIED.,.F.,.F.,(4,1,1,1,1,1,
1,4),(191.637151868977,192.189297563053,193.186940423913,194.184583284772,
195.182226145631,196.179869006491,197.17751186735,197.920337176157),
 .UNSPECIFIED.);
#444=B_SPLINE_CURVE_WITH_KNOTS('',3,(#14723,#14724,#14725,#14726,#14727,
#14728,#14729,#14730,#14731,#14732),.UNSPECIFIED.,.F.,.F.,(4,1,1,1,1,1,
1,4),(191.637151868977,191.94181588113,192.939858162254,193.937900443378,
194.935942724502,195.933985005626,196.93202728675,197.920337176157),
 .UNSPECIFIED.);
#445=B_SPLINE_CURVE_WITH_KNOTS('',3,(#14737,#14738,#14739,#14740,#14741,
#14742,#14743,#14744,#14745,#14746),.UNSPECIFIED.,.F.,.F.,(4,1,1,1,1,1,
1,4),(185.353966561798,186.203440397897,187.201083258756,188.198726119616,
189.196368980475,190.194011841334,191.191654702194,191.637151868977),
 .UNSPECIFIED.);
#446=B_SPLINE_CURVE_WITH_KNOTS('',3,(#14747,#14748,#14749,#14750,#14751,
#14752,#14753,#14754,#14755,#14756),.UNSPECIFIED.,.F.,.F.,(4,1,1,1,1,1,
1,4),(185.353966561798,185.953562194385,186.951604475509,187.949646756633,
188.947689037757,189.945731318881,190.943773600006,191.637151868977),
 .UNSPECIFIED.);
#447=B_SPLINE_CURVE_WITH_KNOTS('',3,(#14761,#14762,#14763,#14764,#14765,
#14766,#14767,#14768,#14769,#14770,#14771),.UNSPECIFIED.,.F.,.F.,(4,1,1,
1,1,1,1,1,4),(179.070781254618,179.219940371881,180.21758323274,181.2152260936,
182.212868954459,183.210511815318,184.208154676178,185.205797537037,185.353966561798),
 .UNSPECIFIED.);
#448=B_SPLINE_CURVE_WITH_KNOTS('',3,(#14772,#14773,#14774,#14775,#14776,
#14777,#14778,#14779,#14780,#14781),.UNSPECIFIED.,.F.,.F.,(4,1,1,1,1,1,
1,4),(179.070781254618,179.965308507641,180.963350788765,181.961393069889,
182.959435351013,183.957477632137,184.955519913261,185.353966561798),
 .UNSPECIFIED.);
#449=B_SPLINE_CURVE_WITH_KNOTS('',3,(#14786,#14787,#14788,#14789,#14790,
#14791,#14792,#14793,#14794,#14795),.UNSPECIFIED.,.F.,.F.,(4,1,1,1,1,1,
1,4),(172.787595947439,173.234083206724,174.231726067584,175.229368928443,
176.227011789303,177.224654650162,178.222297511021,179.070781254618),
 .UNSPECIFIED.);
#450=B_SPLINE_CURVE_WITH_KNOTS('',3,(#14796,#14797,#14798,#14799,#14800,
#14801,#14802,#14803,#14804,#14805,#14806),.UNSPECIFIED.,.F.,.F.,(4,1,1,
1,1,1,1,1,4),(172.787595947439,172.979012539773,173.977054820897,174.975097102021,
175.973139383145,176.971181664269,177.969223945393,178.967266226517,179.070781254618),
 .UNSPECIFIED.);
#451=B_SPLINE_CURVE_WITH_KNOTS('',3,(#14811,#14812,#14813,#14814,#14815,
#14816,#14817,#14818,#14819,#14820),.UNSPECIFIED.,.F.,.F.,(4,1,1,1,1,1,
1,4),(166.504410640259,167.248226041568,168.245868902427,169.243511763287,
170.241154624146,171.238797485006,172.236440345865,172.787595947439),
 .UNSPECIFIED.);
#452=B_SPLINE_CURVE_WITH_KNOTS('',3,(#14821,#14822,#14823,#14824,#14825,
#14826,#14827,#14828,#14829,#14830),.UNSPECIFIED.,.F.,.F.,(4,1,1,1,1,1,
1,4),(166.504410640259,166.990758853029,167.988801134153,168.986843415277,
169.984885696401,170.982927977525,171.980970258649,172.787595947439),
 .UNSPECIFIED.);
#453=B_SPLINE_CURVE_WITH_KNOTS('',3,(#14835,#14836,#14837,#14838,#14839,
#14840,#14841,#14842,#14843,#14844,#14845),.UNSPECIFIED.,.F.,.F.,(4,1,1,
1,1,1,1,1,4),(160.22122533308,160.264726015552,161.262368876412,162.260011737271,
163.25765459813,164.25529745899,165.252940319849,166.250583180709,166.504410640259),
 .UNSPECIFIED.);
#454=B_SPLINE_CURVE_WITH_KNOTS('',3,(#14846,#14847,#14848,#14849,#14850,
#14851,#14852,#14853,#14854,#14855),.UNSPECIFIED.,.F.,.F.,(4,1,1,1,1,1,
1,4),(160.22122533308,161.002505166285,162.000547447409,162.998589728533,
163.996632009657,164.994674290781,165.992716571905,166.504410640259),
 .UNSPECIFIED.);
#455=B_SPLINE_CURVE_WITH_KNOTS('',3,(#14860,#14861,#14862,#14863,#14864,
#14865,#14866,#14867,#14868,#14869),.UNSPECIFIED.,.F.,.F.,(4,1,1,1,1,1,
1,4),(153.9380400259,154.278868850396,155.276511711255,156.274154572115,
157.271797432974,158.269440293833,159.267083154693,160.22122533308),
 .UNSPECIFIED.);
#456=B_SPLINE_CURVE_WITH_KNOTS('',3,(#14870,#14871,#14872,#14873,#14874,
#14875,#14876,#14877,#14878,#14879,#14880),.UNSPECIFIED.,.F.,.F.,(4,1,1,
1,1,1,1,1,4),(153.9380400259,154.016209198417,155.014251479541,156.012293760665,
157.010336041789,158.008378322913,159.006420604037,160.004462885161,160.22122533308),
 .UNSPECIFIED.);
#457=B_SPLINE_CURVE_WITH_KNOTS('',3,(#14885,#14886,#14887,#14888,#14889,
#14890,#14891,#14892,#14893,#14894),.UNSPECIFIED.,.F.,.F.,(4,1,1,1,1,1,
1,4),(147.65485471872,148.293011685239,149.290654546099,150.288297406958,
151.285940267817,152.283583128677,153.281225989536,153.9380400259),
 .UNSPECIFIED.);
#458=B_SPLINE_CURVE_WITH_KNOTS('',3,(#14895,#14896,#14897,#14898,#14899,
#14900,#14901,#14902,#14903,#14904),.UNSPECIFIED.,.F.,.F.,(4,1,1,1,1,1,
1,4),(147.65485471872,148.027955511672,149.025997792796,150.02404007392,
151.022082355044,152.020124636168,153.018166917292,153.9380400259),
 .UNSPECIFIED.);
#459=B_SPLINE_CURVE_WITH_KNOTS('',3,(#14909,#14910,#14911,#14912,#14913,
#14914,#14915,#14916,#14917,#14918),.UNSPECIFIED.,.F.,.F.,(4,1,1,1,1,1,
1,4),(141.371669411541,142.307154520083,143.304797380942,144.302440241802,
145.300083102661,146.29772596352,147.29536882438,147.65485471872),
 .UNSPECIFIED.);
#460=B_SPLINE_CURVE_WITH_KNOTS('',3,(#14919,#14920,#14921,#14922,#14923,
#14924,#14925,#14926,#14927,#14928),.UNSPECIFIED.,.F.,.F.,(4,1,1,1,1,1,
1,4),(141.371669411541,142.039701824928,143.037744106052,144.035786387176,
145.0338286683,146.031870949424,147.029913230548,147.65485471872),
 .UNSPECIFIED.);
#461=B_SPLINE_CURVE_WITH_KNOTS('',3,(#14933,#14934,#14935,#14936,#14937,
#14938,#14939,#14940,#14941,#14942,#14943),.UNSPECIFIED.,.F.,.F.,(4,1,1,
1,1,1,1,1,4),(135.088484104361,135.323654494067,136.321297354926,137.318940215786,
138.316583076645,139.314225937505,140.311868798364,141.309511659223,141.371669411541),
 .UNSPECIFIED.);
#462=B_SPLINE_CURVE_WITH_KNOTS('',3,(#14944,#14945,#14946,#14947,#14948,
#14949,#14950,#14951,#14952,#14953),.UNSPECIFIED.,.F.,.F.,(4,1,1,1,1,1,
1,4),(135.088484104361,136.051448138184,137.049490419308,138.047532700432,
139.045574981556,140.04361726268,141.041659543804,141.371669411541),
 .UNSPECIFIED.);
#463=B_SPLINE_CURVE_WITH_KNOTS('',3,(#14958,#14959,#14960,#14961,#14962,
#14963,#14964,#14965,#14966,#14967),.UNSPECIFIED.,.F.,.F.,(4,1,1,1,1,1,
1,4),(128.805298797182,129.337797328911,130.33544018977,131.333083050629,
132.330725911489,133.328368772348,134.326011633208,135.088484104361),
 .UNSPECIFIED.);
#464=B_SPLINE_CURVE_WITH_KNOTS('',3,(#14968,#14969,#14970,#14971,#14972,
#14973,#14974,#14975,#14976,#14977,#14978),.UNSPECIFIED.,.F.,.F.,(4,1,1,
1,1,1,1,1,4),(128.805298797182,129.065152170316,130.06319445144,131.061236732564,
132.059279013688,133.057321294812,134.055363575936,135.05340585706,135.088484104361),
 .UNSPECIFIED.);
#465=B_SPLINE_CURVE_WITH_KNOTS('',3,(#14983,#14984,#14985,#14986,#14987,
#14988,#14989,#14990,#14991,#14992),.UNSPECIFIED.,.F.,.F.,(4,1,1,1,1,1,
1,4),(122.522113490002,123.351940163754,124.349583024614,125.347225885473,
126.344868746332,127.342511607192,128.340154468051,128.805298797182),
 .UNSPECIFIED.);
#466=B_SPLINE_CURVE_WITH_KNOTS('',3,(#14993,#14994,#14995,#14996,#14997,
#14998,#14999,#15000,#15001,#15002),.UNSPECIFIED.,.F.,.F.,(4,1,1,1,1,1,
1,4),(122.522113490002,123.076898483572,124.074940764696,125.07298304582,
126.071025326944,127.069067608068,128.067109889192,128.805298797182),
 .UNSPECIFIED.);
#467=B_SPLINE_CURVE_WITH_KNOTS('',3,(#15007,#15008,#15009,#15010,#15011,
#15012,#15013,#15014,#15015,#15016,#15017),.UNSPECIFIED.,.F.,.F.,(4,1,1,
1,1,1,1,1,4),(116.238928182823,116.368440137738,117.366082998598,118.363725859457,
119.361368720316,120.359011581176,121.356654442035,122.354297302895,122.522113490002),
 .UNSPECIFIED.);
#468=B_SPLINE_CURVE_WITH_KNOTS('',3,(#15018,#15019,#15020,#15021,#15022,
#15023,#15024,#15025,#15026,#15027),.UNSPECIFIED.,.F.,.F.,(4,1,1,1,1,1,
1,4),(116.238928182823,117.088644796828,118.086687077952,119.084729359076,
120.0827716402,121.080813921324,122.078856202448,122.522113490002),
 .UNSPECIFIED.);
#469=B_SPLINE_CURVE_WITH_KNOTS('',3,(#15032,#15033,#15034,#15035,#15036,
#15037,#15038,#15039,#15040,#15041),.UNSPECIFIED.,.F.,.F.,(4,1,1,1,1,1,
1,4),(109.955742875643,110.382582972582,111.380225833441,112.377868694301,
113.37551155516,114.373154416019,115.370797276879,116.238928182823),
 .UNSPECIFIED.);
#470=B_SPLINE_CURVE_WITH_KNOTS('',3,(#15042,#15043,#15044,#15045,#15046,
#15047,#15048,#15049,#15050,#15051,#15052),.UNSPECIFIED.,.F.,.F.,(4,1,1,
1,1,1,1,1,4),(109.955742875643,110.102348828959,111.100391110083,112.098433391207,
113.096475672331,114.094517953455,115.092560234579,116.090602515703,116.238928182823),
 .UNSPECIFIED.);
#471=B_SPLINE_CURVE_WITH_KNOTS('',3,(#15057,#15058,#15059,#15060,#15061,
#15062,#15063,#15064,#15065,#15066),.UNSPECIFIED.,.F.,.F.,(4,1,1,1,1,1,
1,4),(103.672557568463,104.396725807425,105.394368668285,106.392011529144,
107.389654390004,108.387297250863,109.384940111722,109.955742875643),
 .UNSPECIFIED.);
#472=B_SPLINE_CURVE_WITH_KNOTS('',3,(#15067,#15068,#15069,#15070,#15071,
#15072,#15073,#15074,#15075,#15076),.UNSPECIFIED.,.F.,.F.,(4,1,1,1,1,1,
1,4),(103.672557568463,104.114095142215,105.112137423339,106.110179704463,
107.108221985587,108.106264266711,109.104306547835,109.955742875643),
 .UNSPECIFIED.);
#473=B_SPLINE_CURVE_WITH_KNOTS('',3,(#15081,#15082,#15083,#15084,#15085,
#15086,#15087,#15088,#15089,#15090,#15091),.UNSPECIFIED.,.F.,.F.,(4,1,1,
1,1,1,1,1,4),(97.3893722612837,97.4132257814096,98.410868642269,99.4085115031284,
100.406154363988,101.403797224847,102.401440085707,103.399082946566,103.672557568463),
 .UNSPECIFIED.);
#474=B_SPLINE_CURVE_WITH_KNOTS('',3,(#15092,#15093,#15094,#15095,#15096,
#15097,#15098,#15099,#15100,#15101),.UNSPECIFIED.,.F.,.F.,(4,1,1,1,1,1,
1,4),(97.3893722612838,98.125841455471,99.123883736595,100.121926017719,
101.119968298843,102.118010579967,103.116052861091,103.672557568463),
 .UNSPECIFIED.);
#475=B_SPLINE_CURVE_WITH_KNOTS('',3,(#15106,#15107,#15108,#15109,#15110,
#15111,#15112,#15113,#15114,#15115),.UNSPECIFIED.,.F.,.F.,(4,1,1,1,1,1,
1,4),(91.1061869541041,91.4273686162531,92.4250114771125,93.4226543379719,
94.4202971988313,95.4179400596907,96.4155829205502,97.3893722612837),
 .UNSPECIFIED.);
#476=B_SPLINE_CURVE_WITH_KNOTS('',3,(#15116,#15117,#15118,#15119,#15120,
#15121,#15122,#15123,#15124,#15125,#15126),.UNSPECIFIED.,.F.,.F.,(4,1,1,
1,1,1,1,1,4),(91.1061869541042,91.1395454876028,92.1375877687268,93.1356300498508,
94.1336723309749,95.1317146120989,96.1297568932229,97.127799174347,97.3893722612838),
 .UNSPECIFIED.);
#477=B_SPLINE_CURVE_WITH_KNOTS('',3,(#15131,#15132,#15133,#15134,#15135,
#15136,#15137,#15138,#15139,#15140),.UNSPECIFIED.,.F.,.F.,(4,1,1,1,1,1,
1,4),(84.8230016469245,85.4415114510967,86.4391543119561,87.4367971728155,
88.4344400336749,89.4320828945343,90.4297257553937,91.1061869541041),
 .UNSPECIFIED.);
#478=B_SPLINE_CURVE_WITH_KNOTS('',3,(#15141,#15142,#15143,#15144,#15145,
#15146,#15147,#15148,#15149,#15150),.UNSPECIFIED.,.F.,.F.,(4,1,1,1,1,1,
1,4),(84.8230016469246,85.1512918008586,86.1493340819827,87.1473763631067,
88.1454186442307,89.1434609253548,90.1415032064788,91.1061869541042),
 .UNSPECIFIED.);
#479=B_SPLINE_CURVE_WITH_KNOTS('',3,(#15155,#15156,#15157,#15158,#15159,
#15160,#15161,#15162,#15163,#15164),.UNSPECIFIED.,.F.,.F.,(4,1,1,1,1,1,
1,4),(78.539816339745,79.4556542859402,80.4532971467996,81.4509400076591,
82.4485828685185,83.4462257293779,84.4438685902373,84.8230016469245),
 .UNSPECIFIED.);
#480=B_SPLINE_CURVE_WITH_KNOTS('',3,(#15165,#15166,#15167,#15168,#15169,
#15170,#15171,#15172,#15173,#15174),.UNSPECIFIED.,.F.,.F.,(4,1,1,1,1,1,
1,4),(78.539816339745,79.1630381141145,80.1610803952385,81.1591226763625,
82.1571649574865,83.1552072386106,84.1532495197346,84.8230016469246),
 .UNSPECIFIED.);
#481=B_SPLINE_CURVE_WITH_KNOTS('',3,(#15179,#15180,#15181,#15182,#15183,
#15184,#15185,#15186,#15187,#15188,#15189),.UNSPECIFIED.,.F.,.F.,(4,1,1,
1,1,1,1,1,4),(72.2566310325654,72.4721542599244,73.4697971207838,74.4674399816432,
75.4650828425026,76.462725703362,77.4603685642214,78.4580114250808,78.539816339745),
 .UNSPECIFIED.);
#482=B_SPLINE_CURVE_WITH_KNOTS('',3,(#15190,#15191,#15192,#15193,#15194,
#15195,#15196,#15197,#15198,#15199),.UNSPECIFIED.,.F.,.F.,(4,1,1,1,1,1,
1,4),(72.2566310325654,73.1747844273703,74.1728267084943,75.1708689896184,
76.1689112707424,77.1669535518664,78.1649958329905,78.539816339745),
 .UNSPECIFIED.);
#483=B_SPLINE_CURVE_WITH_KNOTS('',3,(#15204,#15205,#15206,#15207,#15208,
#15209,#15210,#15211,#15212,#15213),.UNSPECIFIED.,.F.,.F.,(4,1,1,1,1,1,
1,4),(65.9734457253858,66.486297094768,67.4839399556274,68.4815828164868,
69.4792256773462,70.4768685382056,71.474511399065,72.2566310325654),
 .UNSPECIFIED.);
#484=B_SPLINE_CURVE_WITH_KNOTS('',3,(#15214,#15215,#15216,#15217,#15218,
#15219,#15220,#15221,#15222,#15223,#15224),.UNSPECIFIED.,.F.,.F.,(4,1,1,
1,1,1,1,1,4),(65.9734457253858,66.1884884595021,67.1865307406262,68.1845730217502,
69.1826153028742,70.1806575839982,71.1786998651223,72.1767421462463,72.2566310325654),
 .UNSPECIFIED.);
#485=B_SPLINE_CURVE_WITH_KNOTS('',3,(#15229,#15230,#15231,#15232,#15233,
#15234,#15235,#15236,#15237,#15238),.UNSPECIFIED.,.F.,.F.,(4,1,1,1,1,1,
1,4),(59.6902604182062,60.5004399296115,61.4980827904709,62.4957256513303,
63.4933685121897,64.4910113730492,65.4886542339086,65.9734457253858),
 .UNSPECIFIED.);
#486=B_SPLINE_CURVE_WITH_KNOTS('',3,(#15239,#15240,#15241,#15242,#15243,
#15244,#15245,#15246,#15247,#15248),.UNSPECIFIED.,.F.,.F.,(4,1,1,1,1,1,
1,4),(59.6902604182062,60.200234772758,61.198277053882,62.196319335006,
63.19436161613,64.1924038972541,65.1904461783781,65.9734457253858),
 .UNSPECIFIED.);
#487=B_SPLINE_CURVE_WITH_KNOTS('',3,(#15253,#15254,#15255,#15256,#15257,
#15258,#15259,#15260,#15261,#15262,#15263),.UNSPECIFIED.,.F.,.F.,(4,1,1,
1,1,1,1,1,4),(53.4070751110266,53.5169399035957,54.5145827644551,55.5122256253145,
56.5098684861739,57.5075113470333,58.5051542078927,59.5027970687521,59.6902604182062),
 .UNSPECIFIED.);
#488=B_SPLINE_CURVE_WITH_KNOTS('',3,(#15264,#15265,#15266,#15267,#15268,
#15269,#15270,#15271,#15272,#15273),.UNSPECIFIED.,.F.,.F.,(4,1,1,1,1,1,
1,4),(53.4070751110266,54.2119810860138,55.2100233671378,56.2080656482619,
57.2061079293859,58.2041502105099,59.2021924916339,59.6902604182062),
 .UNSPECIFIED.);
#489=B_SPLINE_CURVE_WITH_KNOTS('',3,(#15278,#15279,#15280,#15281,#15282,
#15283,#15284,#15285,#15286,#15287),.UNSPECIFIED.,.F.,.F.,(4,1,1,1,1,1,
1,4),(47.123889803847,47.5310827384393,48.5287255992987,49.5263684601581,
50.5240113210175,51.5216541818769,52.5192970427363,53.4070751110266),
 .UNSPECIFIED.);
#490=B_SPLINE_CURVE_WITH_KNOTS('',3,(#15288,#15289,#15290,#15291,#15292,
#15293,#15294,#15295,#15296,#15297,#15298),.UNSPECIFIED.,.F.,.F.,(4,1,1,
1,1,1,1,1,4),(47.123889803847,47.2256851181456,48.2237273992696,49.2217696803937,
50.2198119615177,51.2178542426417,52.2158965237657,53.2139388048898,53.4070751110266),
 .UNSPECIFIED.);
#491=B_SPLINE_CURVE_WITH_KNOTS('',3,(#15303,#15304,#15305,#15306,#15307,
#15308,#15309,#15310,#15311,#15312),.UNSPECIFIED.,.F.,.F.,(4,1,1,1,1,1,
1,4),(40.8407044966674,41.5452255732828,42.5428684341422,43.5405112950016,
44.538154155861,45.5357970167204,46.5334398775799,47.123889803847),
 .UNSPECIFIED.);
#492=B_SPLINE_CURVE_WITH_KNOTS('',3,(#15313,#15314,#15315,#15316,#15317,
#15318,#15319,#15320,#15321,#15322),.UNSPECIFIED.,.F.,.F.,(4,1,1,1,1,1,
1,4),(40.8407044966675,41.2374314314014,42.2354737125255,43.2335159936495,
44.2315582747735,45.2296005558975,46.2276428370216,47.123889803847),
 .UNSPECIFIED.);
#493=B_SPLINE_CURVE_WITH_KNOTS('',3,(#15327,#15328,#15329,#15330,#15331,
#15332,#15333,#15334,#15335,#15336,#15337),.UNSPECIFIED.,.F.,.F.,(4,1,1,
1,1,1,1,1,4),(34.5575191894878,34.561725547267,35.5593684081264,36.5570112689858,
37.5546541298452,38.5522969907046,39.549939851564,40.5475827124234,40.8407044966674),
 .UNSPECIFIED.);
#494=B_SPLINE_CURVE_WITH_KNOTS('',3,(#15338,#15339,#15340,#15341,#15342,
#15343,#15344,#15345,#15346,#15347),.UNSPECIFIED.,.F.,.F.,(4,1,1,1,1,1,
1,4),(34.5575191894879,35.2491777446573,36.2472200257813,37.2452623069053,
38.2433045880294,39.2413468691534,40.2393891502774,40.8407044966675),
 .UNSPECIFIED.);
#495=B_SPLINE_CURVE_WITH_KNOTS('',3,(#15352,#15353,#15354,#15355,#15356,
#15357,#15358,#15359,#15360,#15361),.UNSPECIFIED.,.F.,.F.,(4,1,1,1,1,1,
1,4),(28.2743338823082,28.5758683821105,29.5735112429699,30.5711541038294,
31.5687969646888,32.5664398255482,33.5640826864076,34.5575191894878),
 .UNSPECIFIED.);
#496=B_SPLINE_CURVE_WITH_KNOTS('',3,(#15362,#15363,#15364,#15365,#15366,
#15367,#15368,#15369,#15370,#15371),.UNSPECIFIED.,.F.,.F.,(4,1,1,1,1,1,
1,4),(28.2743338823083,29.2609240579131,30.2589663390371,31.2570086201612,
32.2550509012852,33.2530931824092,34.2511354635333,34.5575191894879),
 .UNSPECIFIED.);
#497=B_SPLINE_CURVE_WITH_KNOTS('',3,(#15376,#15377,#15378,#15379,#15380,
#15381,#15382,#15383,#15384,#15385),.UNSPECIFIED.,.F.,.F.,(4,1,1,1,1,1,
1,4),(21.9911485751286,22.5900112169541,23.5876540778135,24.5852969386729,
25.5829397995323,26.5805826603917,27.5782255212511,28.2743338823082),
 .UNSPECIFIED.);
#498=B_SPLINE_CURVE_WITH_KNOTS('',3,(#15386,#15387,#15388,#15389,#15390,
#15391,#15392,#15393,#15394,#15395,#15396),.UNSPECIFIED.,.F.,.F.,(4,1,1,
1,1,1,1,1,4),(21.9911485751287,22.2746280900449,23.272670371169,24.270712652293,
25.268754933417,26.266797214541,27.2648394956651,28.2628817767891,28.2743338823083),
 .UNSPECIFIED.);
#499=B_SPLINE_CURVE_WITH_KNOTS('',3,(#15401,#15402,#15403,#15404,#15405,
#15406,#15407,#15408,#15409,#15410),.UNSPECIFIED.,.F.,.F.,(4,1,1,1,1,1,
1,4),(15.707963267949,16.6041540517977,17.6017969126571,18.5994397735165,
19.5970826343759,20.5947254952353,21.5923683560947,21.9911485751286),
 .UNSPECIFIED.);
#500=B_SPLINE_CURVE_WITH_KNOTS('',3,(#15411,#15412,#15413,#15414,#15415,
#15416,#15417,#15418,#15419,#15420),.UNSPECIFIED.,.F.,.F.,(4,1,1,1,1,1,
1,4),(15.7079632679491,16.2863744033008,17.2844166844248,18.2824589655488,
19.2805012466728,20.2785435277969,21.2765858089209,21.9911485751287),
 .UNSPECIFIED.);
#501=B_SPLINE_CURVE_WITH_KNOTS('',3,(#15423,#15424,#15425,#15426,#15427,
#15428,#15429,#15430,#15431,#15432,#15433,#15434,#15435,#15436,#15437,#15438,
#15439,#15440,#15441,#15442,#15443,#15444,#15445,#15446,#15447,#15448,#15449,
#15450,#15451,#15452,#15453,#15454,#15455,#15456,#15457,#15458,#15459,#15460,
#15461,#15462,#15463,#15464,#15465,#15466,#15467,#15468,#15469,#15470,#15471,
#15472,#15473,#15474,#15475,#15476,#15477,#15478,#15479,#15480,#15481,#15482,
#15483,#15484,#15485,#15486,#15487,#15488,#15489,#15490,#15491,#15492,#15493,
#15494,#15495,#15496,#15497,#15498,#15499,#15500,#15501,#15502,#15503,#15504,
#15505,#15506,#15507,#15508,#15509,#15510,#15511,#15512,#15513,#15514,#15515,
#15516,#15517,#15518,#15519,#15520,#15521,#15522,#15523,#15524,#15525,#15526,
#15527,#15528,#15529,#15530,#15531,#15532,#15533,#15534,#15535,#15536,#15537,
#15538,#15539,#15540,#15541,#15542,#15543),.UNSPECIFIED.,.F.,.F.,(4,3,3,
3,3,3,3,3,3,3,3,3,3,3,3,3,3,3,3,3,3,3,3,3,3,3,3,3,3,3,3,3,3,3,3,3,3,3,3,
3,4),(-0.753008129282056,-0.726412283548368,-0.715911613874471,-0.694893371653716,
-0.683361029549332,-0.673826434412814,-0.652889016486892,-0.639679181765185,
-0.63195159856097,-0.60480408471638,-0.59150990338668,-0.582561183693184,
-0.554067746128576,-0.540494882749548,-0.528208608719221,-0.505843484121927,
-0.4921308028701,-0.483102814228457,-0.456032674248847,-0.436199115577779,
-0.427073928162626,-0.400948091236321,-0.382860905241332,-0.374822254310016,
-0.34584221065474,-0.333939649620793,-0.324058619604945,-0.29393738163796,
-0.278576588250954,-0.269234263278142,-0.238815915606663,-0.225742435796944,
-0.216239773488962,-0.18666367230127,-0.170750005528772,-0.161294486761502,
-0.129614927749849,-0.114924930935507,-0.106250072717365,-0.0979353687381955,
-0.0965360155478562),.UNSPECIFIED.);
#502=B_SPLINE_CURVE_WITH_KNOTS('',3,(#15545,#15546,#15547,#15548,#15549,
#15550,#15551,#15552,#15553,#15554,#15555,#15556,#15557,#15558,#15559,#15560,
#15561,#15562,#15563,#15564,#15565,#15566,#15567,#15568,#15569,#15570,#15571,
#15572,#15573,#15574,#15575,#15576,#15577,#15578,#15579,#15580,#15581),
 .UNSPECIFIED.,.F.,.F.,(4,3,3,3,3,3,3,3,3,3,3,3,4),(-0.204609524178132,
-0.173922074105667,-0.152149392827302,-0.142793959810126,-0.12983323009626,
-0.11308637627832,-0.0998536142809363,-0.090547498816978,-0.0679106241127335,
-0.0514558350659385,-0.042025593252969,-0.0155529233063705,0.),
 .UNSPECIFIED.);
#503=B_SPLINE_CURVE_WITH_KNOTS('',3,(#15584,#15585,#15586,#15587,#15588,
#15589,#15590,#15591,#15592,#15593,#15594,#15595,#15596,#15597,#15598,#15599),
 .UNSPECIFIED.,.F.,.F.,(4,3,3,3,3,4),(-0.0965360155478562,-0.0724020116608921,
-0.0590232605257019,-0.050388474335024,-0.0186937936910934,0.),
 .UNSPECIFIED.);
#504=B_SPLINE_CURVE_WITH_KNOTS('',3,(#16388,#16389,#16390,#16391,#16392,
#16393,#16394,#16395),.UNSPECIFIED.,.F.,.F.,(4,1,1,1,1,4),(11.6159397475006,
12.61358260836,13.6112254692194,14.6088683300789,15.6065111909383,15.707963267949),
 .UNSPECIFIED.);
#505=B_SPLINE_CURVE_WITH_KNOTS('',3,(#16396,#16397,#16398,#16399,#16400,
#16401,#16402,#16403,#16404,#16405,#16406,#16407,#16408,#16409,#16410,#16411,
#16412,#16413,#16414,#16415,#16416,#16417,#16418,#16419,#16420,#16421,#16422,
#16423,#16424,#16425,#16426,#16427,#16428,#16429,#16430,#16431,#16432,#16433,
#16434,#16435,#16436,#16437,#16438,#16439,#16440,#16441,#16442,#16443,#16444),
 .UNSPECIFIED.,.F.,.F.,(4,3,3,3,3,3,3,3,3,3,3,3,3,3,3,3,4),(-0.275362278356892,
-0.263988733943187,-0.242277787653762,-0.228409792083558,-0.208856161945484,
-0.197709057767663,-0.168075464588018,-0.150222803571495,-0.140083955862437,
-0.125365894046572,-0.0997819296507484,-0.0889593225835958,-0.0667194919376969,
-0.0511923416312717,-0.0404361839568205,-0.0141940669149386,0.),
 .UNSPECIFIED.);
#506=B_SPLINE_CURVE_WITH_KNOTS('',3,(#16445,#16446,#16447,#16448,#16449,
#16450,#16451,#16452,#16453,#16454,#16455,#16456,#16457,#16458,#16459,#16460,
#16461,#16462,#16463),.UNSPECIFIED.,.F.,.F.,(4,3,3,3,3,3,4),(-191.027404416132,
-190.549786424147,-189.552143563287,-188.554500702428,-187.556857841568,
-186.559214980709,-186.304397428656),.UNSPECIFIED.);
#507=B_SPLINE_CURVE_WITH_KNOTS('',3,(#16466,#16467,#16468,#16469,#16470,
#16471,#16472,#16473,#16474),.UNSPECIFIED.,.F.,.F.,(4,1,1,1,1,1,4),(10.3752088276283,
11.2961629976806,12.2942052788047,13.2922475599287,14.2902898410527,15.2883321221767,
15.7079632679491),.UNSPECIFIED.);
#508=B_SPLINE_CURVE_WITH_KNOTS('',3,(#17268,#17269,#17270,#17271,#17272,
#17273,#17274,#17275,#17276,#17277,#17278,#17279,#17280,#17281,#17282,#17283,
#17284,#17285,#17286,#17287,#17288,#17289),.UNSPECIFIED.,.F.,.F.,(4,3,3,
3,3,3,3,4),(183.335115714669,183.639779726821,184.637822007945,185.635864289069,
186.633906570193,187.631948851317,188.629991132441,188.954231742812),
 .UNSPECIFIED.);
#509=B_SPLINE_CURVE_WITH_KNOTS('',3,(#17290,#17291,#17292,#17293,#17294,
#17295,#17296,#17297,#17298,#17299,#17300,#17301,#17302,#17303,#17304,#17305,
#17306,#17307,#17308,#17309,#17310,#17311,#17312,#17313,#17314,#17315,#17316,
#17317,#17318,#17319,#17320,#17321,#17322,#17323,#17324,#17325,#17326,#17327,
#17328,#17329,#17330,#17331,#17332,#17333,#17334,#17335,#17336,#17337,#17338,
#17339,#17340,#17341),.UNSPECIFIED.,.F.,.F.,(4,3,3,3,3,3,3,3,3,3,3,3,3,
3,3,3,3,4),(-0.276631791712714,-0.267404104599176,-0.245529112929484,-0.233826742508505,
-0.212230201958684,-0.201819484750363,-0.173281546649687,-0.162756755581661,
-0.152537502224722,-0.140478169692516,-0.120739781640826,-0.110641775261762,
-0.100726383882944,-0.0755447879122082,-0.0587891884452614,-0.0493012364577666,
-0.0182848522583483,0.),.UNSPECIFIED.);
#510=B_SPLINE_CURVE_WITH_KNOTS('',3,(#17396,#17397,#17398,#17399,#17400,
#17401,#17402),.UNSPECIFIED.,.F.,.F.,(4,3,4),(-30.159289474462,-29.2544199692899,
-28.9853432330879),.UNSPECIFIED.);
#511=B_SPLINE_CURVE_WITH_KNOTS('',3,(#17408,#17409,#17410,#17411,#17412,
#17413,#17414,#17415,#17416,#17417,#17418,#17419,#17420,#17421,#17422,#17423,
#17424,#17425,#17426),.UNSPECIFIED.,.F.,.F.,(4,3,3,3,3,3,4),(26.4423043696954,
27.3041253046706,28.2792726369803,29.25441996929,30.2295673015996,31.2047146339093,
32.179861966219),.UNSPECIFIED.);
#512=B_SPLINE_CURVE_WITH_KNOTS('',3,(#17428,#17429,#17430,#17431,#17432,
#17433,#17434,#17435,#17436,#17437,#17438,#17439,#17440,#17441,#17442,#17443,
#17444,#17445,#17446,#17447,#17448,#17449),.UNSPECIFIED.,.F.,.F.,(4,3,3,
3,3,3,3,4),(-28.9853432330879,-28.2792726369803,-27.3041253046706,-26.3289779723609,
-25.3538306400513,-24.3786833077416,-23.403535975432,-22.7021579259084),
 .UNSPECIFIED.);
#513=B_SPLINE_CURVE_WITH_KNOTS('',3,(#17454,#17455,#17456,#17457,#17458,
#17459,#17460,#17461,#17462,#17463,#17464,#17465,#17466,#17467,#17468,#17469,
#17470,#17471,#17472,#17473,#17474,#17475,#17476,#17477,#17478),
 .UNSPECIFIED.,.F.,.F.,(4,3,3,3,3,3,3,3,4),(20.1591190625159,20.478093978503,
21.4532413108126,22.4283886431223,23.403535975432,24.3786833077416,25.3538306400513,
26.328977972361,26.4423043696954),.UNSPECIFIED.);
#514=B_SPLINE_CURVE_WITH_KNOTS('',3,(#17479,#17480,#17481,#17482,#17483,
#17484,#17485,#17486,#17487,#17488,#17489,#17490,#17491,#17492,#17493,#17494,
#17495,#17496,#17497,#17498,#17499,#17500,#17501,#17502,#17503),
 .UNSPECIFIED.,.F.,.F.,(4,3,3,3,3,3,3,3,4),(-22.7021579259084,-22.4283886431223,
-21.4532413108126,-20.478093978503,-19.5029466461933,-18.5277993138836,
-17.552651981574,-16.5775046492643,-16.4189726187288),.UNSPECIFIED.);
#515=B_SPLINE_CURVE_WITH_KNOTS('',3,(#17508,#17509,#17510,#17511,#17512,
#17513,#17514,#17515,#17516,#17517,#17518,#17519,#17520,#17521,#17522,#17523,
#17524,#17525,#17526,#17527,#17528,#17529),.UNSPECIFIED.,.F.,.F.,(4,3,3,
3,3,3,3,4),(13.8759337553363,14.627209984645,15.6023573169546,16.5775046492643,
17.552651981574,18.5277993138836,19.5029466461933,20.1591190625159),
 .UNSPECIFIED.);
#516=B_SPLINE_CURVE_WITH_KNOTS('',3,(#17530,#17531,#17532,#17533,#17534,
#17535,#17536,#17537,#17538,#17539,#17540,#17541,#17542,#17543,#17544,#17545,
#17546,#17547,#17548,#17549,#17550,#17551),.UNSPECIFIED.,.F.,.F.,(4,3,3,
3,3,3,3,4),(-16.4189726187288,-15.6023573169546,-14.627209984645,-13.6520626523353,
-12.6769153200256,-11.701767987716,-10.7266206554063,-10.1357873115492),
 .UNSPECIFIED.);
#517=B_SPLINE_CURVE_WITH_KNOTS('',3,(#17557,#17558,#17559,#17560,#17561,
#17562,#17563,#17564,#17565,#17566,#17567,#17568,#17569),.UNSPECIFIED.,
 .F.,.F.,(4,3,3,3,4),(-3.8526020043696,-2.92544199692899,-1.95029466461933,
-0.975147332309664,0.),.UNSPECIFIED.);
#518=B_SPLINE_CURVE_WITH_KNOTS('',3,(#17572,#17573,#17574,#17575,#17576,
#17577,#17578,#17579,#17580,#17581,#17582,#17583,#17584,#17585,#17586,#17587,
#17588,#17589,#17590),.UNSPECIFIED.,.F.,.F.,(4,3,3,3,3,3,4),(2.02057249175693,
2.925441996929,3.90058932923866,4.87573666154832,5.85088399385799,6.82603132616766,
7.59274844815668),.UNSPECIFIED.);
#519=B_SPLINE_CURVE_WITH_KNOTS('',3,(#17596,#17597,#17598,#17599,#17600,
#17601,#17602),.UNSPECIFIED.,.F.,.F.,(4,1,1,1,4),(40.8407044966673,41.1097812328693,
42.084928565179,43.0600758974886,44.0352232297983),.UNSPECIFIED.);
#520=B_SPLINE_CURVE_WITH_KNOTS('',3,(#17605,#17606,#17607,#17608,#17609,
#17610,#17611),.UNSPECIFIED.,.F.,.F.,(4,1,1,1,4),(40.8407044966673,41.7025254316425,
42.6776727639522,43.6528200962618,44.5576896014339),.UNSPECIFIED.);
#521=B_SPLINE_CURVE_WITH_KNOTS('',3,(#17616,#17617,#17618,#17619,#17620,
#17621,#17622,#17623,#17624,#17625),.UNSPECIFIED.,.F.,.F.,(4,1,1,1,1,1,
1,4),(34.5575191894877,35.2588972390113,36.234044571321,37.2091919036307,
38.1843392359403,39.15948656825,40.1346339005596,40.8407044966673),
 .UNSPECIFIED.);
#522=B_SPLINE_CURVE_WITH_KNOTS('',3,(#17626,#17627,#17628,#17629,#17630,
#17631,#17632,#17633,#17634,#17635,#17636),.UNSPECIFIED.,.F.,.F.,(4,1,1,
1,1,1,1,1,4),(34.5575191894877,34.8764941054748,35.8516414377845,36.8267887700942,
37.8019361024038,38.7770834347135,39.7522307670232,40.7273780993328,40.8407044966673),
 .UNSPECIFIED.);
#523=B_SPLINE_CURVE_WITH_KNOTS('',3,(#17641,#17642,#17643,#17644,#17645,
#17646,#17647,#17648,#17649,#17650,#17651),.UNSPECIFIED.,.F.,.F.,(4,1,1,
1,1,1,1,1,4),(28.2743338823081,28.4328659128437,29.4080132451533,30.383160577463,
31.3583079097727,32.3334552420823,33.308602574392,34.2837499067017,34.5575191894877),
 .UNSPECIFIED.);
#524=B_SPLINE_CURVE_WITH_KNOTS('',3,(#17652,#17653,#17654,#17655,#17656,
#17657,#17658,#17659,#17660,#17661),.UNSPECIFIED.,.F.,.F.,(4,1,1,1,1,1,
1,4),(28.2743338823081,29.0256101116168,30.0007574439265,30.9759047762362,
31.9510521085458,32.9261994408555,33.9013467731652,34.5575191894877),
 .UNSPECIFIED.);
#525=B_SPLINE_CURVE_WITH_KNOTS('',3,(#17666,#17667,#17668,#17669,#17670,
#17671,#17672,#17673,#17674,#17675),.UNSPECIFIED.,.F.,.F.,(4,1,1,1,1,1,
1,4),(21.9911485751285,22.5819819189857,23.5571292512954,24.532276583605,
25.5074239159147,26.4825712482243,27.457718580534,28.2743338823081),
 .UNSPECIFIED.);
#526=B_SPLINE_CURVE_WITH_KNOTS('',3,(#17676,#17677,#17678,#17679,#17680,
#17681,#17682,#17683,#17684,#17685,#17686),.UNSPECIFIED.,.F.,.F.,(4,1,1,
1,1,1,1,1,4),(21.9911485751285,22.1995787854492,23.1747261177589,24.1498734500685,
25.1250207823782,26.1001681146879,27.0753154469975,28.0504627793072,28.2743338823081),
 .UNSPECIFIED.);
#527=B_SPLINE_CURVE_WITH_KNOTS('',3,(#17692,#17693,#17694,#17695,#17696),
 .UNSPECIFIED.,.F.,.F.,(4,1,4),(14.3984001269719,15.3735474592815,15.7079632679489),
 .UNSPECIFIED.);
#528=B_SPLINE_CURVE_WITH_KNOTS('',3,(#17699,#17700,#17701,#17702,#17703),
 .UNSPECIFIED.,.F.,.F.,(4,1,4),(13.8759337553363,14.7808032605084,15.7079632679489),
 .UNSPECIFIED.);
#529=B_SPLINE_CURVE_WITH_KNOTS('',3,(#17705,#17706,#17707,#17708,#17709,
#17710,#17711,#17712,#17713,#17714,#17715),.UNSPECIFIED.,.F.,.F.,(4,1,1,
1,1,1,1,1,4),(15.7079632679489,15.755950592818,16.7310979251277,17.7062452574374,
18.681392589747,19.6565399220567,20.6316872543664,21.606834586676,21.9911485751285),
 .UNSPECIFIED.);
#530=B_SPLINE_CURVE_WITH_KNOTS('',3,(#17716,#17717,#17718,#17719,#17720,
#17721,#17722,#17723,#17724,#17725),.UNSPECIFIED.,.F.,.F.,(4,1,1,1,1,1,
1,4),(15.7079632679489,16.3486947915912,17.3238421239009,18.2989894562105,
19.2741367885202,20.2492841208299,21.2244314531395,21.9911485751285),
 .UNSPECIFIED.);
#531=B_SPLINE_CURVE_WITH_KNOTS('',3,(#17870,#17871,#17872,#17873,#17874,
#17875,#17876,#17877,#17878,#17879,#17880,#17881,#17882,#17883,#17884,#17885,
#17886,#17887,#17888,#17889,#17890,#17891,#17892,#17893,#17894,#17895,#17896,
#17897,#17898,#17899,#17900,#17901,#17902,#17903,#17904,#17905,#17906,#17907,
#17908,#17909,#17910,#17911,#17912,#17913,#17914,#17915,#17916,#17917,#17918),
 .UNSPECIFIED.,.F.,.F.,(4,3,3,3,3,3,3,3,3,3,3,3,3,3,3,3,4),(0.,0.0320333804888866,
0.0505515708593653,0.0603413132804416,0.0917900141854983,0.108096115778005,
0.122914675479851,0.145143248337739,0.168151513577436,0.177516949333476,
0.202471322707608,0.21794283081622,0.231200110368267,0.247503117401854,
0.263651632124391,0.277334442830003,0.286347380332244),.UNSPECIFIED.);
#532=B_SPLINE_CURVE_WITH_KNOTS('',3,(#17919,#17920,#17921,#17922,#17923,
#17924,#17925,#17926,#17927,#17928,#17929,#17930,#17931,#17932,#17933,#17934,
#17935,#17936,#17937,#17938,#17939,#17940,#17941,#17942,#17943,#17944,#17945,
#17946,#17947,#17948,#17949,#17950,#17951,#17952,#17953,#17954,#17955,#17956,
#17957,#17958,#17959,#17960,#17961,#17962,#17963,#17964,#17965,#17966,#17967),
 .UNSPECIFIED.,.F.,.F.,(4,3,3,3,3,3,3,3,3,3,3,3,3,3,3,3,4),(0.,0.0274305464075637,
0.0492901149097146,0.0591933555873536,0.0887250095166089,0.100015570674795,
0.108381796308415,0.130826479038955,0.152531076563578,0.162815893631175,
0.190691958353668,0.212372986031639,0.222945305605857,0.245534254906135,
0.257847836118801,0.274320152521146,0.28514280399515),.UNSPECIFIED.);
#533=B_SPLINE_CURVE_WITH_KNOTS('',3,(#17968,#17969,#17970,#17971,#17972,
#17973,#17974,#17975,#17976,#17977,#17978,#17979,#17980,#17981,#17982,#17983,
#17984,#17985,#17986,#17987,#17988,#17989,#17990,#17991,#17992),
 .UNSPECIFIED.,.F.,.F.,(4,3,3,3,3,3,3,3,4),(-10.1357873115492,-9.75147332309665,
-8.77632599078699,-7.80117865847732,-6.82603132616766,-5.85088399385799,
-4.87573666154833,-3.90058932923866,-3.8526020043696),.UNSPECIFIED.);
#534=B_SPLINE_CURVE_WITH_KNOTS('',3,(#18137,#18138,#18139,#18140,#18141,
#18142,#18143,#18144,#18145,#18146,#18147,#18148,#18149,#18150,#18151,#18152,
#18153,#18154,#18155,#18156,#18157,#18158,#18159,#18160,#18161,#18162,#18163,
#18164,#18165,#18166,#18167,#18168,#18169,#18170,#18171,#18172,#18173,#18174,
#18175,#18176,#18177,#18178,#18179,#18180,#18181,#18182,#18183,#18184,#18185),
 .UNSPECIFIED.,.F.,.F.,(4,3,3,3,3,3,3,3,3,3,3,3,3,3,3,3,4),(0.,0.0274305890506951,
0.0492901290331875,0.0591933603491513,0.0887250177779717,0.100015607166709,
0.108381835831352,0.13082647903896,0.152531071764912,0.162815892251191,
0.190691957318683,0.212372984486691,0.22294529735758,0.245534140364172,
0.257847701250626,0.274320152521159,0.285142803995162),.UNSPECIFIED.);
#535=B_SPLINE_CURVE_WITH_KNOTS('',3,(#18186,#18187,#18188,#18189,#18190,
#18191,#18192,#18193,#18194,#18195,#18196,#18197,#18198,#18199,#18200,#18201,
#18202,#18203,#18204,#18205,#18206,#18207,#18208,#18209,#18210),
 .UNSPECIFIED.,.F.,.F.,(4,3,3,3,3,3,3,3,4),(7.59274844815668,7.80117865847732,
8.77632599078698,9.75147332309665,10.7266206554063,11.701767987716,12.6769153200256,
13.6520626523353,13.8759337553363),.UNSPECIFIED.);
#536=B_SPLINE_CURVE_WITH_KNOTS('',3,(#18211,#18212,#18213,#18214,#18215,
#18216,#18217,#18218,#18219,#18220,#18221,#18222,#18223,#18224,#18225,#18226,
#18227,#18228,#18229,#18230,#18231,#18232,#18233,#18234,#18235,#18236,#18237,
#18238,#18239,#18240,#18241,#18242,#18243,#18244,#18245,#18246,#18247,#18248,
#18249,#18250,#18251,#18252,#18253,#18254,#18255,#18256,#18257,#18258,#18259),
 .UNSPECIFIED.,.F.,.F.,(4,3,3,3,3,3,3,3,3,3,3,3,3,3,3,3,4),(0.,0.0320334058164849,
0.0505515938322513,0.0603413311462071,0.0917900214840119,0.108096111687201,
0.122914678304232,0.145143248337743,0.168151527562726,0.177516955081398,
0.202471327018552,0.217942288122009,0.231200024743484,0.24750284136614,
0.263651600306541,0.277334442830014,0.286347380332252),.UNSPECIFIED.);
#537=SHAPE_REPRESENTATION_RELATIONSHIP('SRR','None',#18397,#546);
#538=SHAPE_REPRESENTATION_RELATIONSHIP('SRR','None',#18398,#547);
#539=SHAPE_REPRESENTATION_RELATIONSHIP('SRR','None',#18399,#548);
#540=SHAPE_REPRESENTATION_RELATIONSHIP('SRR','None',#18401,#549);
#541=SHAPE_REPRESENTATION_RELATIONSHIP('SRR','None',#18402,#550);
#542=SHAPE_REPRESENTATION_RELATIONSHIP('SRR','None',#18403,#551);
#543=SHAPE_REPRESENTATION_RELATIONSHIP('SRR','None',#18404,#552);
#544=SHAPE_REPRESENTATION_RELATIONSHIP('SRR','None',#18405,#553);
#545=SHAPE_REPRESENTATION_RELATIONSHIP('SRR','None',#18406,#554);
#546=ADVANCED_BREP_SHAPE_REPRESENTATION('',(#564),#18343);
#547=ADVANCED_BREP_SHAPE_REPRESENTATION('',(#565),#18344);
#548=ADVANCED_BREP_SHAPE_REPRESENTATION('',(#566),#18345);
#549=ADVANCED_BREP_SHAPE_REPRESENTATION('',(#567),#18347);
#550=ADVANCED_BREP_SHAPE_REPRESENTATION('',(#568),#18348);
#551=ADVANCED_BREP_SHAPE_REPRESENTATION('',(#569),#18349);
#552=ADVANCED_BREP_SHAPE_REPRESENTATION('',(#570),#18350);
#553=ADVANCED_BREP_SHAPE_REPRESENTATION('',(#571),#18351);
#554=ADVANCED_BREP_SHAPE_REPRESENTATION('',(#572),#18352);
#555=STYLED_ITEM('',(#18456),#564);
#556=STYLED_ITEM('',(#18457),#565);
#557=STYLED_ITEM('',(#18458),#566);
#558=STYLED_ITEM('',(#18459),#567);
#559=STYLED_ITEM('',(#18459),#568);
#560=STYLED_ITEM('',(#18460),#569);
#561=STYLED_ITEM('',(#18458),#570);
#562=STYLED_ITEM('',(#18461),#571);
#563=STYLED_ITEM('',(#18462),#572);
#564=MANIFOLD_SOLID_BREP('Body1',#6486);
#565=MANIFOLD_SOLID_BREP('Body1',#6487);
#566=MANIFOLD_SOLID_BREP('Body1',#6488);
#567=MANIFOLD_SOLID_BREP('Body1',#6489);
#568=MANIFOLD_SOLID_BREP('Body1',#6490);
#569=MANIFOLD_SOLID_BREP('Body1',#6491);
#570=MANIFOLD_SOLID_BREP('Body1',#6492);
#571=MANIFOLD_SOLID_BREP('Body1',#6493);
#572=MANIFOLD_SOLID_BREP('Body1',#6494);
#573=TOROIDAL_SURFACE('',#6634,1.2,0.1);
#574=TOROIDAL_SURFACE('',#6644,1.2,0.1);
#575=FACE_BOUND('',#1173,.T.);
#576=FACE_BOUND('',#1174,.T.);
#577=FACE_BOUND('',#1175,.T.);
#578=FACE_BOUND('',#1176,.T.);
#579=FACE_BOUND('',#1180,.T.);
#580=FACE_BOUND('',#1181,.T.);
#581=FACE_BOUND('',#1182,.T.);
#582=FACE_BOUND('',#1183,.T.);
#583=FACE_BOUND('',#1197,.T.);
#584=FACE_BOUND('',#1199,.T.);
#585=FACE_BOUND('',#1202,.T.);
#586=FACE_BOUND('',#1219,.T.);
#587=FACE_BOUND('',#1222,.T.);
#588=FACE_BOUND('',#1233,.T.);
#589=FACE_BOUND('',#1235,.T.);
#590=FACE_BOUND('',#1247,.T.);
#591=FACE_BOUND('',#1256,.T.);
#592=FACE_BOUND('',#1257,.T.);
#593=FACE_BOUND('',#1258,.T.);
#594=FACE_BOUND('',#1273,.T.);
#595=FACE_BOUND('',#1274,.T.);
#596=FACE_BOUND('',#1275,.T.);
#597=FACE_BOUND('',#1311,.T.);
#598=FACE_BOUND('',#1312,.T.);
#599=FACE_BOUND('',#1313,.T.);
#600=FACE_BOUND('',#1314,.T.);
#601=FACE_BOUND('',#1315,.T.);
#602=FACE_BOUND('',#1316,.T.);
#603=FACE_BOUND('',#1330,.T.);
#604=FACE_BOUND('',#1338,.T.);
#605=FACE_BOUND('',#1349,.T.);
#606=FACE_BOUND('',#1351,.T.);
#607=FACE_BOUND('',#1363,.T.);
#608=FACE_BOUND('',#1372,.T.);
#609=FACE_BOUND('',#1373,.T.);
#610=FACE_BOUND('',#1374,.T.);
#611=FACE_BOUND('',#1389,.T.);
#612=FACE_BOUND('',#1390,.T.);
#613=FACE_BOUND('',#1391,.T.);
#614=FACE_BOUND('',#1427,.T.);
#615=FACE_BOUND('',#1428,.T.);
#616=FACE_BOUND('',#1429,.T.);
#617=FACE_BOUND('',#1430,.T.);
#618=FACE_BOUND('',#1431,.T.);
#619=FACE_BOUND('',#1432,.T.);
#620=FACE_BOUND('',#1438,.T.);
#621=FACE_BOUND('',#1442,.T.);
#622=FACE_BOUND('',#1446,.T.);
#623=FACE_BOUND('',#1450,.T.);
#624=FACE_BOUND('',#1470,.T.);
#625=FACE_BOUND('',#1471,.T.);
#626=FACE_BOUND('',#1476,.T.);
#627=FACE_BOUND('',#1477,.T.);
#628=FACE_BOUND('',#1478,.T.);
#629=FACE_BOUND('',#1479,.T.);
#630=FACE_BOUND('',#1480,.T.);
#631=FACE_BOUND('',#1481,.T.);
#632=FACE_BOUND('',#1556,.T.);
#633=FACE_BOUND('',#1559,.T.);
#634=FACE_BOUND('',#1575,.T.);
#635=FACE_BOUND('',#1584,.T.);
#636=FACE_BOUND('',#1588,.T.);
#637=FACE_BOUND('',#1590,.T.);
#638=CONICAL_SURFACE('',#6607,4.2044765934785,0.927295218001611);
#639=CONICAL_SURFACE('',#7012,0.1,0.785398163397448);
#640=PLANE('',#6606);
#641=PLANE('',#6610);
#642=PLANE('',#6611);
#643=PLANE('',#6612);
#644=PLANE('',#6619);
#645=PLANE('',#6620);
#646=PLANE('',#6621);
#647=PLANE('',#6622);
#648=PLANE('',#6623);
#649=PLANE('',#6630);
#650=PLANE('',#6641);
#651=PLANE('',#6648);
#652=PLANE('',#6649);
#653=PLANE('',#6650);
#654=PLANE('',#6651);
#655=PLANE('',#6652);
#656=PLANE('',#6653);
#657=PLANE('',#6654);
#658=PLANE('',#6655);
#659=PLANE('',#6660);
#660=PLANE('',#6662);
#661=PLANE('',#6666);
#662=PLANE('',#6671);
#663=PLANE('',#6673);
#664=PLANE('',#6675);
#665=PLANE('',#6676);
#666=PLANE('',#6677);
#667=PLANE('',#6684);
#668=PLANE('',#6702);
#669=PLANE('',#6707);
#670=PLANE('',#6713);
#671=PLANE('',#6714);
#672=PLANE('',#6715);
#673=PLANE('',#6716);
#674=PLANE('',#6717);
#675=PLANE('',#6718);
#676=PLANE('',#6719);
#677=PLANE('',#6720);
#678=PLANE('',#6722);
#679=PLANE('',#6724);
#680=PLANE('',#6725);
#681=PLANE('',#6726);
#682=PLANE('',#6727);
#683=PLANE('',#6728);
#684=PLANE('',#6729);
#685=PLANE('',#6730);
#686=PLANE('',#6731);
#687=PLANE('',#6732);
#688=PLANE('',#6733);
#689=PLANE('',#6734);
#690=PLANE('',#6739);
#691=PLANE('',#6741);
#692=PLANE('',#6742);
#693=PLANE('',#6743);
#694=PLANE('',#6744);
#695=PLANE('',#6745);
#696=PLANE('',#6746);
#697=PLANE('',#6747);
#698=PLANE('',#6749);
#699=PLANE('',#6766);
#700=PLANE('',#6785);
#701=PLANE('',#6786);
#702=PLANE('',#6787);
#703=PLANE('',#6801);
#704=PLANE('',#6802);
#705=PLANE('',#6803);
#706=PLANE('',#6804);
#707=PLANE('',#6805);
#708=PLANE('',#6806);
#709=PLANE('',#6807);
#710=PLANE('',#6809);
#711=PLANE('',#6810);
#712=PLANE('',#6811);
#713=PLANE('',#6812);
#714=PLANE('',#6813);
#715=PLANE('',#6814);
#716=PLANE('',#6815);
#717=PLANE('',#6821);
#718=PLANE('',#6822);
#719=PLANE('',#6823);
#720=PLANE('',#6824);
#721=PLANE('',#6825);
#722=PLANE('',#6826);
#723=PLANE('',#6827);
#724=PLANE('',#6828);
#725=PLANE('',#6830);
#726=PLANE('',#6832);
#727=PLANE('',#6833);
#728=PLANE('',#6834);
#729=PLANE('',#6835);
#730=PLANE('',#6836);
#731=PLANE('',#6837);
#732=PLANE('',#6838);
#733=PLANE('',#6839);
#734=PLANE('',#6840);
#735=PLANE('',#6841);
#736=PLANE('',#6842);
#737=PLANE('',#6847);
#738=PLANE('',#6849);
#739=PLANE('',#6850);
#740=PLANE('',#6851);
#741=PLANE('',#6852);
#742=PLANE('',#6853);
#743=PLANE('',#6854);
#744=PLANE('',#6855);
#745=PLANE('',#6857);
#746=PLANE('',#6874);
#747=PLANE('',#6893);
#748=PLANE('',#6894);
#749=PLANE('',#6895);
#750=PLANE('',#6903);
#751=PLANE('',#6908);
#752=PLANE('',#6909);
#753=PLANE('',#6914);
#754=PLANE('',#6915);
#755=PLANE('',#6920);
#756=PLANE('',#6921);
#757=PLANE('',#6926);
#758=PLANE('',#6945);
#759=PLANE('',#6946);
#760=PLANE('',#6947);
#761=PLANE('',#6948);
#762=PLANE('',#7018);
#763=PLANE('',#7019);
#764=PLANE('',#7020);
#765=PLANE('',#7021);
#766=PLANE('',#7022);
#767=PLANE('',#7023);
#768=PLANE('',#7024);
#769=PLANE('',#7025);
#770=PLANE('',#7029);
#771=PLANE('',#7030);
#772=PLANE('',#7048);
#773=PLANE('',#7050);
#774=PLANE('',#7051);
#775=PLANE('',#7052);
#776=PLANE('',#7053);
#777=PLANE('',#7054);
#778=PLANE('',#7055);
#779=PLANE('',#7056);
#780=PLANE('',#7072);
#781=PLANE('',#7073);
#782=FACE_OUTER_BOUND('',#1155,.T.);
#783=FACE_OUTER_BOUND('',#1156,.T.);
#784=FACE_OUTER_BOUND('',#1157,.T.);
#785=FACE_OUTER_BOUND('',#1158,.T.);
#786=FACE_OUTER_BOUND('',#1159,.T.);
#787=FACE_OUTER_BOUND('',#1160,.T.);
#788=FACE_OUTER_BOUND('',#1161,.T.);
#789=FACE_OUTER_BOUND('',#1162,.T.);
#790=FACE_OUTER_BOUND('',#1163,.T.);
#791=FACE_OUTER_BOUND('',#1164,.T.);
#792=FACE_OUTER_BOUND('',#1165,.T.);
#793=FACE_OUTER_BOUND('',#1166,.T.);
#794=FACE_OUTER_BOUND('',#1167,.T.);
#795=FACE_OUTER_BOUND('',#1168,.T.);
#796=FACE_OUTER_BOUND('',#1169,.T.);
#797=FACE_OUTER_BOUND('',#1170,.T.);
#798=FACE_OUTER_BOUND('',#1171,.T.);
#799=FACE_OUTER_BOUND('',#1172,.T.);
#800=FACE_OUTER_BOUND('',#1177,.T.);
#801=FACE_OUTER_BOUND('',#1178,.T.);
#802=FACE_OUTER_BOUND('',#1179,.T.);
#803=FACE_OUTER_BOUND('',#1184,.T.);
#804=FACE_OUTER_BOUND('',#1185,.T.);
#805=FACE_OUTER_BOUND('',#1186,.T.);
#806=FACE_OUTER_BOUND('',#1187,.T.);
#807=FACE_OUTER_BOUND('',#1188,.T.);
#808=FACE_OUTER_BOUND('',#1189,.T.);
#809=FACE_OUTER_BOUND('',#1190,.T.);
#810=FACE_OUTER_BOUND('',#1191,.T.);
#811=FACE_OUTER_BOUND('',#1192,.T.);
#812=FACE_OUTER_BOUND('',#1193,.T.);
#813=FACE_OUTER_BOUND('',#1194,.T.);
#814=FACE_OUTER_BOUND('',#1195,.T.);
#815=FACE_OUTER_BOUND('',#1196,.T.);
#816=FACE_OUTER_BOUND('',#1198,.T.);
#817=FACE_OUTER_BOUND('',#1200,.T.);
#818=FACE_OUTER_BOUND('',#1201,.T.);
#819=FACE_OUTER_BOUND('',#1203,.T.);
#820=FACE_OUTER_BOUND('',#1204,.T.);
#821=FACE_OUTER_BOUND('',#1205,.T.);
#822=FACE_OUTER_BOUND('',#1206,.T.);
#823=FACE_OUTER_BOUND('',#1207,.T.);
#824=FACE_OUTER_BOUND('',#1208,.T.);
#825=FACE_OUTER_BOUND('',#1209,.T.);
#826=FACE_OUTER_BOUND('',#1210,.T.);
#827=FACE_OUTER_BOUND('',#1211,.T.);
#828=FACE_OUTER_BOUND('',#1212,.T.);
#829=FACE_OUTER_BOUND('',#1213,.T.);
#830=FACE_OUTER_BOUND('',#1214,.T.);
#831=FACE_OUTER_BOUND('',#1215,.T.);
#832=FACE_OUTER_BOUND('',#1216,.T.);
#833=FACE_OUTER_BOUND('',#1217,.T.);
#834=FACE_OUTER_BOUND('',#1218,.T.);
#835=FACE_OUTER_BOUND('',#1220,.T.);
#836=FACE_OUTER_BOUND('',#1221,.T.);
#837=FACE_OUTER_BOUND('',#1223,.T.);
#838=FACE_OUTER_BOUND('',#1224,.T.);
#839=FACE_OUTER_BOUND('',#1225,.T.);
#840=FACE_OUTER_BOUND('',#1226,.T.);
#841=FACE_OUTER_BOUND('',#1227,.T.);
#842=FACE_OUTER_BOUND('',#1228,.T.);
#843=FACE_OUTER_BOUND('',#1229,.T.);
#844=FACE_OUTER_BOUND('',#1230,.T.);
#845=FACE_OUTER_BOUND('',#1231,.T.);
#846=FACE_OUTER_BOUND('',#1232,.T.);
#847=FACE_OUTER_BOUND('',#1234,.T.);
#848=FACE_OUTER_BOUND('',#1236,.T.);
#849=FACE_OUTER_BOUND('',#1237,.T.);
#850=FACE_OUTER_BOUND('',#1238,.T.);
#851=FACE_OUTER_BOUND('',#1239,.T.);
#852=FACE_OUTER_BOUND('',#1240,.T.);
#853=FACE_OUTER_BOUND('',#1241,.T.);
#854=FACE_OUTER_BOUND('',#1242,.T.);
#855=FACE_OUTER_BOUND('',#1243,.T.);
#856=FACE_OUTER_BOUND('',#1244,.T.);
#857=FACE_OUTER_BOUND('',#1245,.T.);
#858=FACE_OUTER_BOUND('',#1246,.T.);
#859=FACE_OUTER_BOUND('',#1248,.T.);
#860=FACE_OUTER_BOUND('',#1249,.T.);
#861=FACE_OUTER_BOUND('',#1250,.T.);
#862=FACE_OUTER_BOUND('',#1251,.T.);
#863=FACE_OUTER_BOUND('',#1252,.T.);
#864=FACE_OUTER_BOUND('',#1253,.T.);
#865=FACE_OUTER_BOUND('',#1254,.T.);
#866=FACE_OUTER_BOUND('',#1255,.T.);
#867=FACE_OUTER_BOUND('',#1259,.T.);
#868=FACE_OUTER_BOUND('',#1260,.T.);
#869=FACE_OUTER_BOUND('',#1261,.T.);
#870=FACE_OUTER_BOUND('',#1262,.T.);
#871=FACE_OUTER_BOUND('',#1263,.T.);
#872=FACE_OUTER_BOUND('',#1264,.T.);
#873=FACE_OUTER_BOUND('',#1265,.T.);
#874=FACE_OUTER_BOUND('',#1266,.T.);
#875=FACE_OUTER_BOUND('',#1267,.T.);
#876=FACE_OUTER_BOUND('',#1268,.T.);
#877=FACE_OUTER_BOUND('',#1269,.T.);
#878=FACE_OUTER_BOUND('',#1270,.T.);
#879=FACE_OUTER_BOUND('',#1271,.T.);
#880=FACE_OUTER_BOUND('',#1272,.T.);
#881=FACE_OUTER_BOUND('',#1276,.T.);
#882=FACE_OUTER_BOUND('',#1277,.T.);
#883=FACE_OUTER_BOUND('',#1278,.T.);
#884=FACE_OUTER_BOUND('',#1279,.T.);
#885=FACE_OUTER_BOUND('',#1280,.T.);
#886=FACE_OUTER_BOUND('',#1281,.T.);
#887=FACE_OUTER_BOUND('',#1282,.T.);
#888=FACE_OUTER_BOUND('',#1283,.T.);
#889=FACE_OUTER_BOUND('',#1284,.T.);
#890=FACE_OUTER_BOUND('',#1285,.T.);
#891=FACE_OUTER_BOUND('',#1286,.T.);
#892=FACE_OUTER_BOUND('',#1287,.T.);
#893=FACE_OUTER_BOUND('',#1288,.T.);
#894=FACE_OUTER_BOUND('',#1289,.T.);
#895=FACE_OUTER_BOUND('',#1290,.T.);
#896=FACE_OUTER_BOUND('',#1291,.T.);
#897=FACE_OUTER_BOUND('',#1292,.T.);
#898=FACE_OUTER_BOUND('',#1293,.T.);
#899=FACE_OUTER_BOUND('',#1294,.T.);
#900=FACE_OUTER_BOUND('',#1295,.T.);
#901=FACE_OUTER_BOUND('',#1296,.T.);
#902=FACE_OUTER_BOUND('',#1297,.T.);
#903=FACE_OUTER_BOUND('',#1298,.T.);
#904=FACE_OUTER_BOUND('',#1299,.T.);
#905=FACE_OUTER_BOUND('',#1300,.T.);
#906=FACE_OUTER_BOUND('',#1301,.T.);
#907=FACE_OUTER_BOUND('',#1302,.T.);
#908=FACE_OUTER_BOUND('',#1303,.T.);
#909=FACE_OUTER_BOUND('',#1304,.T.);
#910=FACE_OUTER_BOUND('',#1305,.T.);
#911=FACE_OUTER_BOUND('',#1306,.T.);
#912=FACE_OUTER_BOUND('',#1307,.T.);
#913=FACE_OUTER_BOUND('',#1308,.T.);
#914=FACE_OUTER_BOUND('',#1309,.T.);
#915=FACE_OUTER_BOUND('',#1310,.T.);
#916=FACE_OUTER_BOUND('',#1317,.T.);
#917=FACE_OUTER_BOUND('',#1318,.T.);
#918=FACE_OUTER_BOUND('',#1319,.T.);
#919=FACE_OUTER_BOUND('',#1320,.T.);
#920=FACE_OUTER_BOUND('',#1321,.T.);
#921=FACE_OUTER_BOUND('',#1322,.T.);
#922=FACE_OUTER_BOUND('',#1323,.T.);
#923=FACE_OUTER_BOUND('',#1324,.T.);
#924=FACE_OUTER_BOUND('',#1325,.T.);
#925=FACE_OUTER_BOUND('',#1326,.T.);
#926=FACE_OUTER_BOUND('',#1327,.T.);
#927=FACE_OUTER_BOUND('',#1328,.T.);
#928=FACE_OUTER_BOUND('',#1329,.T.);
#929=FACE_OUTER_BOUND('',#1331,.T.);
#930=FACE_OUTER_BOUND('',#1332,.T.);
#931=FACE_OUTER_BOUND('',#1333,.T.);
#932=FACE_OUTER_BOUND('',#1334,.T.);
#933=FACE_OUTER_BOUND('',#1335,.T.);
#934=FACE_OUTER_BOUND('',#1336,.T.);
#935=FACE_OUTER_BOUND('',#1337,.T.);
#936=FACE_OUTER_BOUND('',#1339,.T.);
#937=FACE_OUTER_BOUND('',#1340,.T.);
#938=FACE_OUTER_BOUND('',#1341,.T.);
#939=FACE_OUTER_BOUND('',#1342,.T.);
#940=FACE_OUTER_BOUND('',#1343,.T.);
#941=FACE_OUTER_BOUND('',#1344,.T.);
#942=FACE_OUTER_BOUND('',#1345,.T.);
#943=FACE_OUTER_BOUND('',#1346,.T.);
#944=FACE_OUTER_BOUND('',#1347,.T.);
#945=FACE_OUTER_BOUND('',#1348,.T.);
#946=FACE_OUTER_BOUND('',#1350,.T.);
#947=FACE_OUTER_BOUND('',#1352,.T.);
#948=FACE_OUTER_BOUND('',#1353,.T.);
#949=FACE_OUTER_BOUND('',#1354,.T.);
#950=FACE_OUTER_BOUND('',#1355,.T.);
#951=FACE_OUTER_BOUND('',#1356,.T.);
#952=FACE_OUTER_BOUND('',#1357,.T.);
#953=FACE_OUTER_BOUND('',#1358,.T.);
#954=FACE_OUTER_BOUND('',#1359,.T.);
#955=FACE_OUTER_BOUND('',#1360,.T.);
#956=FACE_OUTER_BOUND('',#1361,.T.);
#957=FACE_OUTER_BOUND('',#1362,.T.);
#958=FACE_OUTER_BOUND('',#1364,.T.);
#959=FACE_OUTER_BOUND('',#1365,.T.);
#960=FACE_OUTER_BOUND('',#1366,.T.);
#961=FACE_OUTER_BOUND('',#1367,.T.);
#962=FACE_OUTER_BOUND('',#1368,.T.);
#963=FACE_OUTER_BOUND('',#1369,.T.);
#964=FACE_OUTER_BOUND('',#1370,.T.);
#965=FACE_OUTER_BOUND('',#1371,.T.);
#966=FACE_OUTER_BOUND('',#1375,.T.);
#967=FACE_OUTER_BOUND('',#1376,.T.);
#968=FACE_OUTER_BOUND('',#1377,.T.);
#969=FACE_OUTER_BOUND('',#1378,.T.);
#970=FACE_OUTER_BOUND('',#1379,.T.);
#971=FACE_OUTER_BOUND('',#1380,.T.);
#972=FACE_OUTER_BOUND('',#1381,.T.);
#973=FACE_OUTER_BOUND('',#1382,.T.);
#974=FACE_OUTER_BOUND('',#1383,.T.);
#975=FACE_OUTER_BOUND('',#1384,.T.);
#976=FACE_OUTER_BOUND('',#1385,.T.);
#977=FACE_OUTER_BOUND('',#1386,.T.);
#978=FACE_OUTER_BOUND('',#1387,.T.);
#979=FACE_OUTER_BOUND('',#1388,.T.);
#980=FACE_OUTER_BOUND('',#1392,.T.);
#981=FACE_OUTER_BOUND('',#1393,.T.);
#982=FACE_OUTER_BOUND('',#1394,.T.);
#983=FACE_OUTER_BOUND('',#1395,.T.);
#984=FACE_OUTER_BOUND('',#1396,.T.);
#985=FACE_OUTER_BOUND('',#1397,.T.);
#986=FACE_OUTER_BOUND('',#1398,.T.);
#987=FACE_OUTER_BOUND('',#1399,.T.);
#988=FACE_OUTER_BOUND('',#1400,.T.);
#989=FACE_OUTER_BOUND('',#1401,.T.);
#990=FACE_OUTER_BOUND('',#1402,.T.);
#991=FACE_OUTER_BOUND('',#1403,.T.);
#992=FACE_OUTER_BOUND('',#1404,.T.);
#993=FACE_OUTER_BOUND('',#1405,.T.);
#994=FACE_OUTER_BOUND('',#1406,.T.);
#995=FACE_OUTER_BOUND('',#1407,.T.);
#996=FACE_OUTER_BOUND('',#1408,.T.);
#997=FACE_OUTER_BOUND('',#1409,.T.);
#998=FACE_OUTER_BOUND('',#1410,.T.);
#999=FACE_OUTER_BOUND('',#1411,.T.);
#1000=FACE_OUTER_BOUND('',#1412,.T.);
#1001=FACE_OUTER_BOUND('',#1413,.T.);
#1002=FACE_OUTER_BOUND('',#1414,.T.);
#1003=FACE_OUTER_BOUND('',#1415,.T.);
#1004=FACE_OUTER_BOUND('',#1416,.T.);
#1005=FACE_OUTER_BOUND('',#1417,.T.);
#1006=FACE_OUTER_BOUND('',#1418,.T.);
#1007=FACE_OUTER_BOUND('',#1419,.T.);
#1008=FACE_OUTER_BOUND('',#1420,.T.);
#1009=FACE_OUTER_BOUND('',#1421,.T.);
#1010=FACE_OUTER_BOUND('',#1422,.T.);
#1011=FACE_OUTER_BOUND('',#1423,.T.);
#1012=FACE_OUTER_BOUND('',#1424,.T.);
#1013=FACE_OUTER_BOUND('',#1425,.T.);
#1014=FACE_OUTER_BOUND('',#1426,.T.);
#1015=FACE_OUTER_BOUND('',#1433,.T.);
#1016=FACE_OUTER_BOUND('',#1434,.T.);
#1017=FACE_OUTER_BOUND('',#1435,.T.);
#1018=FACE_OUTER_BOUND('',#1436,.T.);
#1019=FACE_OUTER_BOUND('',#1437,.T.);
#1020=FACE_OUTER_BOUND('',#1439,.T.);
#1021=FACE_OUTER_BOUND('',#1440,.T.);
#1022=FACE_OUTER_BOUND('',#1441,.T.);
#1023=FACE_OUTER_BOUND('',#1443,.T.);
#1024=FACE_OUTER_BOUND('',#1444,.T.);
#1025=FACE_OUTER_BOUND('',#1445,.T.);
#1026=FACE_OUTER_BOUND('',#1447,.T.);
#1027=FACE_OUTER_BOUND('',#1448,.T.);
#1028=FACE_OUTER_BOUND('',#1449,.T.);
#1029=FACE_OUTER_BOUND('',#1451,.T.);
#1030=FACE_OUTER_BOUND('',#1452,.T.);
#1031=FACE_OUTER_BOUND('',#1453,.T.);
#1032=FACE_OUTER_BOUND('',#1454,.T.);
#1033=FACE_OUTER_BOUND('',#1455,.T.);
#1034=FACE_OUTER_BOUND('',#1456,.T.);
#1035=FACE_OUTER_BOUND('',#1457,.T.);
#1036=FACE_OUTER_BOUND('',#1458,.T.);
#1037=FACE_OUTER_BOUND('',#1459,.T.);
#1038=FACE_OUTER_BOUND('',#1460,.T.);
#1039=FACE_OUTER_BOUND('',#1461,.T.);
#1040=FACE_OUTER_BOUND('',#1462,.T.);
#1041=FACE_OUTER_BOUND('',#1463,.T.);
#1042=FACE_OUTER_BOUND('',#1464,.T.);
#1043=FACE_OUTER_BOUND('',#1465,.T.);
#1044=FACE_OUTER_BOUND('',#1466,.T.);
#1045=FACE_OUTER_BOUND('',#1467,.T.);
#1046=FACE_OUTER_BOUND('',#1468,.T.);
#1047=FACE_OUTER_BOUND('',#1469,.T.);
#1048=FACE_OUTER_BOUND('',#1472,.T.);
#1049=FACE_OUTER_BOUND('',#1473,.T.);
#1050=FACE_OUTER_BOUND('',#1474,.T.);
#1051=FACE_OUTER_BOUND('',#1475,.T.);
#1052=FACE_OUTER_BOUND('',#1482,.T.);
#1053=FACE_OUTER_BOUND('',#1483,.T.);
#1054=FACE_OUTER_BOUND('',#1484,.T.);
#1055=FACE_OUTER_BOUND('',#1485,.T.);
#1056=FACE_OUTER_BOUND('',#1486,.T.);
#1057=FACE_OUTER_BOUND('',#1487,.T.);
#1058=FACE_OUTER_BOUND('',#1488,.T.);
#1059=FACE_OUTER_BOUND('',#1489,.T.);
#1060=FACE_OUTER_BOUND('',#1490,.T.);
#1061=FACE_OUTER_BOUND('',#1491,.T.);
#1062=FACE_OUTER_BOUND('',#1492,.T.);
#1063=FACE_OUTER_BOUND('',#1493,.T.);
#1064=FACE_OUTER_BOUND('',#1494,.T.);
#1065=FACE_OUTER_BOUND('',#1495,.T.);
#1066=FACE_OUTER_BOUND('',#1496,.T.);
#1067=FACE_OUTER_BOUND('',#1497,.T.);
#1068=FACE_OUTER_BOUND('',#1498,.T.);
#1069=FACE_OUTER_BOUND('',#1499,.T.);
#1070=FACE_OUTER_BOUND('',#1500,.T.);
#1071=FACE_OUTER_BOUND('',#1501,.T.);
#1072=FACE_OUTER_BOUND('',#1502,.T.);
#1073=FACE_OUTER_BOUND('',#1503,.T.);
#1074=FACE_OUTER_BOUND('',#1504,.T.);
#1075=FACE_OUTER_BOUND('',#1505,.T.);
#1076=FACE_OUTER_BOUND('',#1506,.T.);
#1077=FACE_OUTER_BOUND('',#1507,.T.);
#1078=FACE_OUTER_BOUND('',#1508,.T.);
#1079=FACE_OUTER_BOUND('',#1509,.T.);
#1080=FACE_OUTER_BOUND('',#1510,.T.);
#1081=FACE_OUTER_BOUND('',#1511,.T.);
#1082=FACE_OUTER_BOUND('',#1512,.T.);
#1083=FACE_OUTER_BOUND('',#1513,.T.);
#1084=FACE_OUTER_BOUND('',#1514,.T.);
#1085=FACE_OUTER_BOUND('',#1515,.T.);
#1086=FACE_OUTER_BOUND('',#1516,.T.);
#1087=FACE_OUTER_BOUND('',#1517,.T.);
#1088=FACE_OUTER_BOUND('',#1518,.T.);
#1089=FACE_OUTER_BOUND('',#1519,.T.);
#1090=FACE_OUTER_BOUND('',#1520,.T.);
#1091=FACE_OUTER_BOUND('',#1521,.T.);
#1092=FACE_OUTER_BOUND('',#1522,.T.);
#1093=FACE_OUTER_BOUND('',#1523,.T.);
#1094=FACE_OUTER_BOUND('',#1524,.T.);
#1095=FACE_OUTER_BOUND('',#1525,.T.);
#1096=FACE_OUTER_BOUND('',#1526,.T.);
#1097=FACE_OUTER_BOUND('',#1527,.T.);
#1098=FACE_OUTER_BOUND('',#1528,.T.);
#1099=FACE_OUTER_BOUND('',#1529,.T.);
#1100=FACE_OUTER_BOUND('',#1530,.T.);
#1101=FACE_OUTER_BOUND('',#1531,.T.);
#1102=FACE_OUTER_BOUND('',#1532,.T.);
#1103=FACE_OUTER_BOUND('',#1533,.T.);
#1104=FACE_OUTER_BOUND('',#1534,.T.);
#1105=FACE_OUTER_BOUND('',#1535,.T.);
#1106=FACE_OUTER_BOUND('',#1536,.T.);
#1107=FACE_OUTER_BOUND('',#1537,.T.);
#1108=FACE_OUTER_BOUND('',#1538,.T.);
#1109=FACE_OUTER_BOUND('',#1539,.T.);
#1110=FACE_OUTER_BOUND('',#1540,.T.);
#1111=FACE_OUTER_BOUND('',#1541,.T.);
#1112=FACE_OUTER_BOUND('',#1542,.T.);
#1113=FACE_OUTER_BOUND('',#1543,.T.);
#1114=FACE_OUTER_BOUND('',#1544,.T.);
#1115=FACE_OUTER_BOUND('',#1545,.T.);
#1116=FACE_OUTER_BOUND('',#1546,.T.);
#1117=FACE_OUTER_BOUND('',#1547,.T.);
#1118=FACE_OUTER_BOUND('',#1548,.T.);
#1119=FACE_OUTER_BOUND('',#1549,.T.);
#1120=FACE_OUTER_BOUND('',#1550,.T.);
#1121=FACE_OUTER_BOUND('',#1551,.T.);
#1122=FACE_OUTER_BOUND('',#1552,.T.);
#1123=FACE_OUTER_BOUND('',#1553,.T.);
#1124=FACE_OUTER_BOUND('',#1554,.T.);
#1125=FACE_OUTER_BOUND('',#1555,.T.);
#1126=FACE_OUTER_BOUND('',#1557,.T.);
#1127=FACE_OUTER_BOUND('',#1558,.T.);
#1128=FACE_OUTER_BOUND('',#1560,.T.);
#1129=FACE_OUTER_BOUND('',#1561,.T.);
#1130=FACE_OUTER_BOUND('',#1562,.T.);
#1131=FACE_OUTER_BOUND('',#1563,.T.);
#1132=FACE_OUTER_BOUND('',#1564,.T.);
#1133=FACE_OUTER_BOUND('',#1565,.T.);
#1134=FACE_OUTER_BOUND('',#1566,.T.);
#1135=FACE_OUTER_BOUND('',#1567,.T.);
#1136=FACE_OUTER_BOUND('',#1568,.T.);
#1137=FACE_OUTER_BOUND('',#1569,.T.);
#1138=FACE_OUTER_BOUND('',#1570,.T.);
#1139=FACE_OUTER_BOUND('',#1571,.T.);
#1140=FACE_OUTER_BOUND('',#1572,.T.);
#1141=FACE_OUTER_BOUND('',#1573,.T.);
#1142=FACE_OUTER_BOUND('',#1574,.T.);
#1143=FACE_OUTER_BOUND('',#1576,.T.);
#1144=FACE_OUTER_BOUND('',#1577,.T.);
#1145=FACE_OUTER_BOUND('',#1578,.T.);
#1146=FACE_OUTER_BOUND('',#1579,.T.);
#1147=FACE_OUTER_BOUND('',#1580,.T.);
#1148=FACE_OUTER_BOUND('',#1581,.T.);
#1149=FACE_OUTER_BOUND('',#1582,.T.);
#1150=FACE_OUTER_BOUND('',#1583,.T.);
#1151=FACE_OUTER_BOUND('',#1585,.T.);
#1152=FACE_OUTER_BOUND('',#1586,.T.);
#1153=FACE_OUTER_BOUND('',#1587,.T.);
#1154=FACE_OUTER_BOUND('',#1589,.T.);
#1155=EDGE_LOOP('',(#4108,#4109,#4110,#4111));
#1156=EDGE_LOOP('',(#4112,#4113,#4114,#4115));
#1157=EDGE_LOOP('',(#4116,#4117,#4118,#4119));
#1158=EDGE_LOOP('',(#4120,#4121,#4122));
#1159=EDGE_LOOP('',(#4123,#4124,#4125,#4126));
#1160=EDGE_LOOP('',(#4127,#4128,#4129));
#1161=EDGE_LOOP('',(#4130,#4131,#4132,#4133));
#1162=EDGE_LOOP('',(#4134,#4135,#4136,#4137));
#1163=EDGE_LOOP('',(#4138,#4139,#4140,#4141));
#1164=EDGE_LOOP('',(#4142,#4143,#4144,#4145));
#1165=EDGE_LOOP('',(#4146,#4147,#4148,#4149,#4150,#4151,#4152,#4153,#4154));
#1166=EDGE_LOOP('',(#4155,#4156,#4157,#4158,#4159,#4160));
#1167=EDGE_LOOP('',(#4161,#4162,#4163,#4164,#4165,#4166));
#1168=EDGE_LOOP('',(#4167,#4168,#4169,#4170));
#1169=EDGE_LOOP('',(#4171,#4172,#4173,#4174));
#1170=EDGE_LOOP('',(#4175,#4176,#4177,#4178));
#1171=EDGE_LOOP('',(#4179,#4180,#4181,#4182));
#1172=EDGE_LOOP('',(#4183,#4184,#4185,#4186,#4187,#4188,#4189,#4190,#4191,
#4192,#4193,#4194,#4195,#4196,#4197,#4198));
#1173=EDGE_LOOP('',(#4199));
#1174=EDGE_LOOP('',(#4200));
#1175=EDGE_LOOP('',(#4201));
#1176=EDGE_LOOP('',(#4202));
#1177=EDGE_LOOP('',(#4203,#4204,#4205,#4206));
#1178=EDGE_LOOP('',(#4207,#4208,#4209,#4210,#4211));
#1179=EDGE_LOOP('',(#4212,#4213,#4214,#4215,#4216,#4217,#4218,#4219,#4220,
#4221,#4222,#4223,#4224,#4225,#4226,#4227,#4228,#4229,#4230,#4231,#4232));
#1180=EDGE_LOOP('',(#4233));
#1181=EDGE_LOOP('',(#4234));
#1182=EDGE_LOOP('',(#4235));
#1183=EDGE_LOOP('',(#4236));
#1184=EDGE_LOOP('',(#4237,#4238,#4239,#4240,#4241));
#1185=EDGE_LOOP('',(#4242,#4243,#4244,#4245));
#1186=EDGE_LOOP('',(#4246,#4247,#4248,#4249));
#1187=EDGE_LOOP('',(#4250,#4251,#4252,#4253));
#1188=EDGE_LOOP('',(#4254,#4255,#4256,#4257));
#1189=EDGE_LOOP('',(#4258,#4259,#4260,#4261));
#1190=EDGE_LOOP('',(#4262,#4263,#4264,#4265));
#1191=EDGE_LOOP('',(#4266,#4267,#4268,#4269));
#1192=EDGE_LOOP('',(#4270,#4271,#4272,#4273));
#1193=EDGE_LOOP('',(#4274,#4275,#4276,#4277));
#1194=EDGE_LOOP('',(#4278,#4279,#4280,#4281));
#1195=EDGE_LOOP('',(#4282,#4283,#4284,#4285));
#1196=EDGE_LOOP('',(#4286));
#1197=EDGE_LOOP('',(#4287));
#1198=EDGE_LOOP('',(#4288));
#1199=EDGE_LOOP('',(#4289));
#1200=EDGE_LOOP('',(#4290,#4291,#4292,#4293));
#1201=EDGE_LOOP('',(#4294));
#1202=EDGE_LOOP('',(#4295));
#1203=EDGE_LOOP('',(#4296,#4297,#4298,#4299));
#1204=EDGE_LOOP('',(#4300));
#1205=EDGE_LOOP('',(#4301,#4302,#4303,#4304));
#1206=EDGE_LOOP('',(#4305));
#1207=EDGE_LOOP('',(#4306,#4307,#4308,#4309));
#1208=EDGE_LOOP('',(#4310,#4311,#4312,#4313));
#1209=EDGE_LOOP('',(#4314,#4315,#4316,#4317));
#1210=EDGE_LOOP('',(#4318,#4319,#4320,#4321));
#1211=EDGE_LOOP('',(#4322,#4323,#4324,#4325));
#1212=EDGE_LOOP('',(#4326,#4327,#4328,#4329));
#1213=EDGE_LOOP('',(#4330,#4331,#4332,#4333));
#1214=EDGE_LOOP('',(#4334,#4335,#4336,#4337));
#1215=EDGE_LOOP('',(#4338,#4339,#4340,#4341));
#1216=EDGE_LOOP('',(#4342,#4343,#4344,#4345));
#1217=EDGE_LOOP('',(#4346,#4347,#4348,#4349));
#1218=EDGE_LOOP('',(#4350));
#1219=EDGE_LOOP('',(#4351));
#1220=EDGE_LOOP('',(#4352,#4353,#4354,#4355));
#1221=EDGE_LOOP('',(#4356));
#1222=EDGE_LOOP('',(#4357));
#1223=EDGE_LOOP('',(#4358,#4359,#4360,#4361));
#1224=EDGE_LOOP('',(#4362,#4363,#4364,#4365));
#1225=EDGE_LOOP('',(#4366,#4367,#4368,#4369));
#1226=EDGE_LOOP('',(#4370,#4371,#4372,#4373));
#1227=EDGE_LOOP('',(#4374,#4375,#4376,#4377));
#1228=EDGE_LOOP('',(#4378,#4379,#4380,#4381));
#1229=EDGE_LOOP('',(#4382,#4383,#4384,#4385));
#1230=EDGE_LOOP('',(#4386,#4387,#4388,#4389));
#1231=EDGE_LOOP('',(#4390,#4391,#4392,#4393));
#1232=EDGE_LOOP('',(#4394));
#1233=EDGE_LOOP('',(#4395));
#1234=EDGE_LOOP('',(#4396));
#1235=EDGE_LOOP('',(#4397));
#1236=EDGE_LOOP('',(#4398,#4399,#4400,#4401));
#1237=EDGE_LOOP('',(#4402,#4403,#4404,#4405));
#1238=EDGE_LOOP('',(#4406,#4407,#4408,#4409));
#1239=EDGE_LOOP('',(#4410,#4411,#4412,#4413));
#1240=EDGE_LOOP('',(#4414,#4415,#4416,#4417));
#1241=EDGE_LOOP('',(#4418,#4419,#4420,#4421,#4422,#4423));
#1242=EDGE_LOOP('',(#4424,#4425,#4426,#4427,#4428,#4429,#4430,#4431,#4432,
#4433));
#1243=EDGE_LOOP('',(#4434,#4435,#4436,#4437,#4438,#4439,#4440,#4441,#4442,
#4443));
#1244=EDGE_LOOP('',(#4444,#4445,#4446,#4447,#4448,#4449,#4450,#4451,#4452,
#4453));
#1245=EDGE_LOOP('',(#4454,#4455,#4456,#4457,#4458,#4459,#4460,#4461));
#1246=EDGE_LOOP('',(#4462,#4463,#4464,#4465,#4466,#4467,#4468,#4469,#4470,
#4471,#4472,#4473,#4474,#4475,#4476,#4477,#4478,#4479,#4480,#4481,#4482,
#4483,#4484,#4485,#4486,#4487,#4488,#4489,#4490,#4491,#4492,#4493,#4494,
#4495,#4496,#4497,#4498,#4499,#4500,#4501,#4502,#4503));
#1247=EDGE_LOOP('',(#4504,#4505,#4506,#4507,#4508,#4509));
#1248=EDGE_LOOP('',(#4510,#4511,#4512,#4513));
#1249=EDGE_LOOP('',(#4514,#4515,#4516,#4517));
#1250=EDGE_LOOP('',(#4518,#4519,#4520,#4521,#4522,#4523));
#1251=EDGE_LOOP('',(#4524,#4525,#4526,#4527));
#1252=EDGE_LOOP('',(#4528,#4529,#4530,#4531));
#1253=EDGE_LOOP('',(#4532,#4533,#4534,#4535));
#1254=EDGE_LOOP('',(#4536,#4537,#4538,#4539));
#1255=EDGE_LOOP('',(#4540,#4541,#4542,#4543));
#1256=EDGE_LOOP('',(#4544));
#1257=EDGE_LOOP('',(#4545));
#1258=EDGE_LOOP('',(#4546));
#1259=EDGE_LOOP('',(#4547,#4548,#4549,#4550));
#1260=EDGE_LOOP('',(#4551,#4552,#4553,#4554));
#1261=EDGE_LOOP('',(#4555,#4556,#4557,#4558));
#1262=EDGE_LOOP('',(#4559,#4560,#4561,#4562));
#1263=EDGE_LOOP('',(#4563,#4564,#4565,#4566,#4567,#4568,#4569,#4570,#4571,
#4572));
#1264=EDGE_LOOP('',(#4573,#4574,#4575,#4576));
#1265=EDGE_LOOP('',(#4577,#4578,#4579,#4580));
#1266=EDGE_LOOP('',(#4581,#4582,#4583,#4584));
#1267=EDGE_LOOP('',(#4585,#4586,#4587,#4588));
#1268=EDGE_LOOP('',(#4589,#4590,#4591,#4592));
#1269=EDGE_LOOP('',(#4593,#4594,#4595,#4596,#4597,#4598,#4599,#4600,#4601,
#4602));
#1270=EDGE_LOOP('',(#4603,#4604,#4605,#4606));
#1271=EDGE_LOOP('',(#4607,#4608,#4609,#4610));
#1272=EDGE_LOOP('',(#4611,#4612,#4613,#4614));
#1273=EDGE_LOOP('',(#4615));
#1274=EDGE_LOOP('',(#4616));
#1275=EDGE_LOOP('',(#4617));
#1276=EDGE_LOOP('',(#4618,#4619,#4620,#4621));
#1277=EDGE_LOOP('',(#4622,#4623,#4624,#4625));
#1278=EDGE_LOOP('',(#4626,#4627,#4628,#4629,#4630,#4631,#4632,#4633,#4634,
#4635));
#1279=EDGE_LOOP('',(#4636,#4637,#4638,#4639));
#1280=EDGE_LOOP('',(#4640,#4641,#4642,#4643));
#1281=EDGE_LOOP('',(#4644,#4645,#4646,#4647));
#1282=EDGE_LOOP('',(#4648,#4649,#4650,#4651));
#1283=EDGE_LOOP('',(#4652,#4653,#4654,#4655));
#1284=EDGE_LOOP('',(#4656,#4657,#4658));
#1285=EDGE_LOOP('',(#4659,#4660,#4661));
#1286=EDGE_LOOP('',(#4662,#4663,#4664));
#1287=EDGE_LOOP('',(#4665,#4666,#4667,#4668));
#1288=EDGE_LOOP('',(#4669,#4670,#4671,#4672));
#1289=EDGE_LOOP('',(#4673,#4674,#4675));
#1290=EDGE_LOOP('',(#4676,#4677,#4678,#4679));
#1291=EDGE_LOOP('',(#4680,#4681,#4682,#4683));
#1292=EDGE_LOOP('',(#4684,#4685,#4686,#4687));
#1293=EDGE_LOOP('',(#4688,#4689,#4690,#4691));
#1294=EDGE_LOOP('',(#4692,#4693,#4694,#4695));
#1295=EDGE_LOOP('',(#4696,#4697,#4698,#4699));
#1296=EDGE_LOOP('',(#4700,#4701,#4702));
#1297=EDGE_LOOP('',(#4703,#4704,#4705));
#1298=EDGE_LOOP('',(#4706,#4707,#4708));
#1299=EDGE_LOOP('',(#4709,#4710,#4711,#4712));
#1300=EDGE_LOOP('',(#4713,#4714,#4715,#4716));
#1301=EDGE_LOOP('',(#4717,#4718,#4719));
#1302=EDGE_LOOP('',(#4720,#4721,#4722,#4723));
#1303=EDGE_LOOP('',(#4724,#4725,#4726,#4727));
#1304=EDGE_LOOP('',(#4728,#4729,#4730,#4731));
#1305=EDGE_LOOP('',(#4732,#4733,#4734,#4735));
#1306=EDGE_LOOP('',(#4736,#4737,#4738,#4739));
#1307=EDGE_LOOP('',(#4740,#4741,#4742,#4743));
#1308=EDGE_LOOP('',(#4744,#4745,#4746,#4747));
#1309=EDGE_LOOP('',(#4748,#4749,#4750,#4751,#4752,#4753,#4754,#4755));
#1310=EDGE_LOOP('',(#4756,#4757,#4758,#4759));
#1311=EDGE_LOOP('',(#4760));
#1312=EDGE_LOOP('',(#4761));
#1313=EDGE_LOOP('',(#4762));
#1314=EDGE_LOOP('',(#4763));
#1315=EDGE_LOOP('',(#4764));
#1316=EDGE_LOOP('',(#4765));
#1317=EDGE_LOOP('',(#4766,#4767,#4768,#4769));
#1318=EDGE_LOOP('',(#4770,#4771,#4772,#4773));
#1319=EDGE_LOOP('',(#4774,#4775,#4776,#4777));
#1320=EDGE_LOOP('',(#4778,#4779,#4780,#4781));
#1321=EDGE_LOOP('',(#4782,#4783,#4784,#4785));
#1322=EDGE_LOOP('',(#4786,#4787,#4788,#4789));
#1323=EDGE_LOOP('',(#4790,#4791,#4792,#4793));
#1324=EDGE_LOOP('',(#4794,#4795,#4796,#4797));
#1325=EDGE_LOOP('',(#4798,#4799,#4800,#4801));
#1326=EDGE_LOOP('',(#4802,#4803,#4804,#4805));
#1327=EDGE_LOOP('',(#4806,#4807,#4808,#4809));
#1328=EDGE_LOOP('',(#4810,#4811,#4812,#4813));
#1329=EDGE_LOOP('',(#4814,#4815,#4816,#4817,#4818,#4819));
#1330=EDGE_LOOP('',(#4820));
#1331=EDGE_LOOP('',(#4821,#4822,#4823,#4824));
#1332=EDGE_LOOP('',(#4825,#4826,#4827,#4828));
#1333=EDGE_LOOP('',(#4829,#4830,#4831,#4832));
#1334=EDGE_LOOP('',(#4833,#4834,#4835,#4836));
#1335=EDGE_LOOP('',(#4837,#4838,#4839,#4840));
#1336=EDGE_LOOP('',(#4841,#4842,#4843,#4844));
#1337=EDGE_LOOP('',(#4845,#4846,#4847,#4848,#4849,#4850));
#1338=EDGE_LOOP('',(#4851));
#1339=EDGE_LOOP('',(#4852,#4853,#4854,#4855));
#1340=EDGE_LOOP('',(#4856,#4857,#4858,#4859));
#1341=EDGE_LOOP('',(#4860,#4861,#4862,#4863));
#1342=EDGE_LOOP('',(#4864,#4865,#4866,#4867));
#1343=EDGE_LOOP('',(#4868,#4869,#4870,#4871));
#1344=EDGE_LOOP('',(#4872,#4873,#4874,#4875));
#1345=EDGE_LOOP('',(#4876,#4877,#4878,#4879));
#1346=EDGE_LOOP('',(#4880,#4881,#4882,#4883));
#1347=EDGE_LOOP('',(#4884,#4885,#4886,#4887));
#1348=EDGE_LOOP('',(#4888));
#1349=EDGE_LOOP('',(#4889));
#1350=EDGE_LOOP('',(#4890));
#1351=EDGE_LOOP('',(#4891));
#1352=EDGE_LOOP('',(#4892,#4893,#4894,#4895));
#1353=EDGE_LOOP('',(#4896,#4897,#4898,#4899));
#1354=EDGE_LOOP('',(#4900,#4901,#4902,#4903));
#1355=EDGE_LOOP('',(#4904,#4905,#4906,#4907));
#1356=EDGE_LOOP('',(#4908,#4909,#4910,#4911));
#1357=EDGE_LOOP('',(#4912,#4913,#4914,#4915,#4916,#4917));
#1358=EDGE_LOOP('',(#4918,#4919,#4920,#4921,#4922,#4923,#4924,#4925,#4926,
#4927));
#1359=EDGE_LOOP('',(#4928,#4929,#4930,#4931,#4932,#4933,#4934,#4935,#4936,
#4937));
#1360=EDGE_LOOP('',(#4938,#4939,#4940,#4941,#4942,#4943,#4944,#4945,#4946,
#4947));
#1361=EDGE_LOOP('',(#4948,#4949,#4950,#4951,#4952,#4953,#4954,#4955));
#1362=EDGE_LOOP('',(#4956,#4957,#4958,#4959,#4960,#4961,#4962,#4963,#4964,
#4965,#4966,#4967,#4968,#4969,#4970,#4971,#4972,#4973,#4974,#4975,#4976,
#4977,#4978,#4979,#4980,#4981,#4982,#4983,#4984,#4985,#4986,#4987,#4988,
#4989,#4990,#4991,#4992,#4993,#4994,#4995,#4996,#4997));
#1363=EDGE_LOOP('',(#4998,#4999,#5000,#5001,#5002,#5003));
#1364=EDGE_LOOP('',(#5004,#5005,#5006,#5007));
#1365=EDGE_LOOP('',(#5008,#5009,#5010,#5011));
#1366=EDGE_LOOP('',(#5012,#5013,#5014,#5015,#5016,#5017));
#1367=EDGE_LOOP('',(#5018,#5019,#5020,#5021));
#1368=EDGE_LOOP('',(#5022,#5023,#5024,#5025));
#1369=EDGE_LOOP('',(#5026,#5027,#5028,#5029));
#1370=EDGE_LOOP('',(#5030,#5031,#5032,#5033));
#1371=EDGE_LOOP('',(#5034,#5035,#5036,#5037));
#1372=EDGE_LOOP('',(#5038));
#1373=EDGE_LOOP('',(#5039));
#1374=EDGE_LOOP('',(#5040));
#1375=EDGE_LOOP('',(#5041,#5042,#5043,#5044));
#1376=EDGE_LOOP('',(#5045,#5046,#5047,#5048));
#1377=EDGE_LOOP('',(#5049,#5050,#5051,#5052));
#1378=EDGE_LOOP('',(#5053,#5054,#5055,#5056));
#1379=EDGE_LOOP('',(#5057,#5058,#5059,#5060,#5061,#5062,#5063,#5064,#5065,
#5066));
#1380=EDGE_LOOP('',(#5067,#5068,#5069,#5070));
#1381=EDGE_LOOP('',(#5071,#5072,#5073,#5074));
#1382=EDGE_LOOP('',(#5075,#5076,#5077,#5078));
#1383=EDGE_LOOP('',(#5079,#5080,#5081,#5082));
#1384=EDGE_LOOP('',(#5083,#5084,#5085,#5086));
#1385=EDGE_LOOP('',(#5087,#5088,#5089,#5090,#5091,#5092,#5093,#5094,#5095,
#5096));
#1386=EDGE_LOOP('',(#5097,#5098,#5099,#5100));
#1387=EDGE_LOOP('',(#5101,#5102,#5103,#5104));
#1388=EDGE_LOOP('',(#5105,#5106,#5107,#5108));
#1389=EDGE_LOOP('',(#5109));
#1390=EDGE_LOOP('',(#5110));
#1391=EDGE_LOOP('',(#5111));
#1392=EDGE_LOOP('',(#5112,#5113,#5114,#5115));
#1393=EDGE_LOOP('',(#5116,#5117,#5118,#5119));
#1394=EDGE_LOOP('',(#5120,#5121,#5122,#5123,#5124,#5125,#5126,#5127,#5128,
#5129));
#1395=EDGE_LOOP('',(#5130,#5131,#5132,#5133));
#1396=EDGE_LOOP('',(#5134,#5135,#5136,#5137));
#1397=EDGE_LOOP('',(#5138,#5139,#5140,#5141));
#1398=EDGE_LOOP('',(#5142,#5143,#5144,#5145));
#1399=EDGE_LOOP('',(#5146,#5147,#5148,#5149));
#1400=EDGE_LOOP('',(#5150,#5151,#5152));
#1401=EDGE_LOOP('',(#5153,#5154,#5155));
#1402=EDGE_LOOP('',(#5156,#5157,#5158));
#1403=EDGE_LOOP('',(#5159,#5160,#5161,#5162));
#1404=EDGE_LOOP('',(#5163,#5164,#5165,#5166));
#1405=EDGE_LOOP('',(#5167,#5168,#5169));
#1406=EDGE_LOOP('',(#5170,#5171,#5172,#5173));
#1407=EDGE_LOOP('',(#5174,#5175,#5176,#5177));
#1408=EDGE_LOOP('',(#5178,#5179,#5180,#5181));
#1409=EDGE_LOOP('',(#5182,#5183,#5184,#5185));
#1410=EDGE_LOOP('',(#5186,#5187,#5188,#5189));
#1411=EDGE_LOOP('',(#5190,#5191,#5192,#5193));
#1412=EDGE_LOOP('',(#5194,#5195,#5196));
#1413=EDGE_LOOP('',(#5197,#5198,#5199));
#1414=EDGE_LOOP('',(#5200,#5201,#5202));
#1415=EDGE_LOOP('',(#5203,#5204,#5205,#5206));
#1416=EDGE_LOOP('',(#5207,#5208,#5209,#5210));
#1417=EDGE_LOOP('',(#5211,#5212,#5213));
#1418=EDGE_LOOP('',(#5214,#5215,#5216,#5217));
#1419=EDGE_LOOP('',(#5218,#5219,#5220,#5221));
#1420=EDGE_LOOP('',(#5222,#5223,#5224,#5225));
#1421=EDGE_LOOP('',(#5226,#5227,#5228,#5229));
#1422=EDGE_LOOP('',(#5230,#5231,#5232,#5233));
#1423=EDGE_LOOP('',(#5234,#5235,#5236,#5237));
#1424=EDGE_LOOP('',(#5238,#5239,#5240,#5241));
#1425=EDGE_LOOP('',(#5242,#5243,#5244,#5245,#5246,#5247,#5248,#5249));
#1426=EDGE_LOOP('',(#5250,#5251,#5252,#5253));
#1427=EDGE_LOOP('',(#5254,#5255,#5256,#5257,#5258,#5259));
#1428=EDGE_LOOP('',(#5260,#5261,#5262,#5263,#5264,#5265));
#1429=EDGE_LOOP('',(#5266));
#1430=EDGE_LOOP('',(#5267));
#1431=EDGE_LOOP('',(#5268));
#1432=EDGE_LOOP('',(#5269));
#1433=EDGE_LOOP('',(#5270,#5271,#5272,#5273));
#1434=EDGE_LOOP('',(#5274,#5275,#5276,#5277));
#1435=EDGE_LOOP('',(#5278,#5279,#5280,#5281));
#1436=EDGE_LOOP('',(#5282,#5283,#5284,#5285));
#1437=EDGE_LOOP('',(#5286));
#1438=EDGE_LOOP('',(#5287));
#1439=EDGE_LOOP('',(#5288,#5289,#5290,#5291));
#1440=EDGE_LOOP('',(#5292));
#1441=EDGE_LOOP('',(#5293));
#1442=EDGE_LOOP('',(#5294));
#1443=EDGE_LOOP('',(#5295,#5296,#5297,#5298));
#1444=EDGE_LOOP('',(#5299));
#1445=EDGE_LOOP('',(#5300));
#1446=EDGE_LOOP('',(#5301));
#1447=EDGE_LOOP('',(#5302,#5303,#5304,#5305));
#1448=EDGE_LOOP('',(#5306));
#1449=EDGE_LOOP('',(#5307));
#1450=EDGE_LOOP('',(#5308));
#1451=EDGE_LOOP('',(#5309,#5310,#5311,#5312));
#1452=EDGE_LOOP('',(#5313));
#1453=EDGE_LOOP('',(#5314,#5315,#5316,#5317));
#1454=EDGE_LOOP('',(#5318,#5319,#5320,#5321));
#1455=EDGE_LOOP('',(#5322,#5323,#5324,#5325));
#1456=EDGE_LOOP('',(#5326,#5327,#5328,#5329));
#1457=EDGE_LOOP('',(#5330,#5331,#5332,#5333));
#1458=EDGE_LOOP('',(#5334,#5335,#5336,#5337));
#1459=EDGE_LOOP('',(#5338,#5339,#5340,#5341));
#1460=EDGE_LOOP('',(#5342,#5343,#5344,#5345));
#1461=EDGE_LOOP('',(#5346,#5347,#5348,#5349));
#1462=EDGE_LOOP('',(#5350,#5351,#5352,#5353));
#1463=EDGE_LOOP('',(#5354,#5355,#5356,#5357));
#1464=EDGE_LOOP('',(#5358,#5359,#5360,#5361));
#1465=EDGE_LOOP('',(#5362,#5363,#5364,#5365));
#1466=EDGE_LOOP('',(#5366,#5367,#5368,#5369));
#1467=EDGE_LOOP('',(#5370,#5371,#5372,#5373));
#1468=EDGE_LOOP('',(#5374,#5375,#5376,#5377));
#1469=EDGE_LOOP('',(#5378,#5379,#5380,#5381,#5382,#5383,#5384,#5385));
#1470=EDGE_LOOP('',(#5386));
#1471=EDGE_LOOP('',(#5387));
#1472=EDGE_LOOP('',(#5388,#5389,#5390,#5391));
#1473=EDGE_LOOP('',(#5392,#5393,#5394,#5395));
#1474=EDGE_LOOP('',(#5396,#5397,#5398,#5399));
#1475=EDGE_LOOP('',(#5400,#5401,#5402,#5403,#5404,#5405,#5406,#5407));
#1476=EDGE_LOOP('',(#5408));
#1477=EDGE_LOOP('',(#5409));
#1478=EDGE_LOOP('',(#5410));
#1479=EDGE_LOOP('',(#5411));
#1480=EDGE_LOOP('',(#5412));
#1481=EDGE_LOOP('',(#5413));
#1482=EDGE_LOOP('',(#5414,#5415,#5416,#5417));
#1483=EDGE_LOOP('',(#5418,#5419,#5420,#5421));
#1484=EDGE_LOOP('',(#5422,#5423,#5424,#5425));
#1485=EDGE_LOOP('',(#5426,#5427,#5428,#5429));
#1486=EDGE_LOOP('',(#5430,#5431,#5432,#5433));
#1487=EDGE_LOOP('',(#5434,#5435,#5436,#5437));
#1488=EDGE_LOOP('',(#5438,#5439,#5440,#5441));
#1489=EDGE_LOOP('',(#5442,#5443,#5444,#5445));
#1490=EDGE_LOOP('',(#5446,#5447,#5448,#5449));
#1491=EDGE_LOOP('',(#5450,#5451,#5452,#5453));
#1492=EDGE_LOOP('',(#5454,#5455,#5456,#5457));
#1493=EDGE_LOOP('',(#5458,#5459,#5460,#5461));
#1494=EDGE_LOOP('',(#5462,#5463,#5464,#5465));
#1495=EDGE_LOOP('',(#5466,#5467,#5468,#5469));
#1496=EDGE_LOOP('',(#5470,#5471,#5472,#5473));
#1497=EDGE_LOOP('',(#5474,#5475,#5476,#5477));
#1498=EDGE_LOOP('',(#5478,#5479,#5480,#5481));
#1499=EDGE_LOOP('',(#5482,#5483,#5484,#5485));
#1500=EDGE_LOOP('',(#5486,#5487,#5488,#5489));
#1501=EDGE_LOOP('',(#5490,#5491,#5492,#5493));
#1502=EDGE_LOOP('',(#5494,#5495,#5496,#5497));
#1503=EDGE_LOOP('',(#5498,#5499,#5500,#5501));
#1504=EDGE_LOOP('',(#5502,#5503,#5504,#5505));
#1505=EDGE_LOOP('',(#5506,#5507,#5508,#5509));
#1506=EDGE_LOOP('',(#5510,#5511,#5512,#5513));
#1507=EDGE_LOOP('',(#5514,#5515,#5516,#5517));
#1508=EDGE_LOOP('',(#5518,#5519,#5520,#5521));
#1509=EDGE_LOOP('',(#5522,#5523,#5524,#5525));
#1510=EDGE_LOOP('',(#5526,#5527,#5528,#5529));
#1511=EDGE_LOOP('',(#5530,#5531,#5532,#5533));
#1512=EDGE_LOOP('',(#5534,#5535,#5536,#5537));
#1513=EDGE_LOOP('',(#5538,#5539,#5540,#5541));
#1514=EDGE_LOOP('',(#5542,#5543,#5544,#5545));
#1515=EDGE_LOOP('',(#5546,#5547,#5548,#5549));
#1516=EDGE_LOOP('',(#5550,#5551,#5552,#5553));
#1517=EDGE_LOOP('',(#5554,#5555,#5556,#5557));
#1518=EDGE_LOOP('',(#5558,#5559,#5560,#5561));
#1519=EDGE_LOOP('',(#5562,#5563,#5564,#5565));
#1520=EDGE_LOOP('',(#5566,#5567,#5568,#5569));
#1521=EDGE_LOOP('',(#5570,#5571,#5572,#5573));
#1522=EDGE_LOOP('',(#5574,#5575,#5576,#5577));
#1523=EDGE_LOOP('',(#5578,#5579,#5580,#5581));
#1524=EDGE_LOOP('',(#5582,#5583,#5584,#5585));
#1525=EDGE_LOOP('',(#5586,#5587,#5588,#5589));
#1526=EDGE_LOOP('',(#5590,#5591,#5592,#5593));
#1527=EDGE_LOOP('',(#5594,#5595,#5596,#5597));
#1528=EDGE_LOOP('',(#5598,#5599,#5600,#5601));
#1529=EDGE_LOOP('',(#5602,#5603,#5604,#5605));
#1530=EDGE_LOOP('',(#5606,#5607,#5608,#5609));
#1531=EDGE_LOOP('',(#5610,#5611,#5612,#5613));
#1532=EDGE_LOOP('',(#5614,#5615,#5616,#5617));
#1533=EDGE_LOOP('',(#5618,#5619,#5620,#5621));
#1534=EDGE_LOOP('',(#5622,#5623,#5624,#5625));
#1535=EDGE_LOOP('',(#5626,#5627,#5628,#5629));
#1536=EDGE_LOOP('',(#5630,#5631,#5632,#5633));
#1537=EDGE_LOOP('',(#5634,#5635,#5636,#5637));
#1538=EDGE_LOOP('',(#5638,#5639,#5640,#5641));
#1539=EDGE_LOOP('',(#5642,#5643,#5644,#5645));
#1540=EDGE_LOOP('',(#5646,#5647,#5648,#5649));
#1541=EDGE_LOOP('',(#5650,#5651,#5652,#5653));
#1542=EDGE_LOOP('',(#5654,#5655,#5656,#5657));
#1543=EDGE_LOOP('',(#5658,#5659,#5660,#5661,#5662,#5663,#5664,#5665));
#1544=EDGE_LOOP('',(#5666,#5667,#5668,#5669,#5670,#5671,#5672,#5673,#5674,
#5675,#5676,#5677,#5678,#5679,#5680,#5681,#5682,#5683,#5684,#5685,#5686,
#5687,#5688,#5689,#5690,#5691,#5692,#5693,#5694,#5695,#5696,#5697,#5698,
#5699,#5700,#5701,#5702,#5703,#5704,#5705,#5706,#5707,#5708,#5709,#5710,
#5711,#5712,#5713,#5714,#5715,#5716,#5717,#5718,#5719,#5720,#5721,#5722,
#5723,#5724,#5725,#5726,#5727,#5728,#5729));
#1545=EDGE_LOOP('',(#5730,#5731,#5732,#5733));
#1546=EDGE_LOOP('',(#5734,#5735,#5736,#5737,#5738,#5739,#5740,#5741,#5742,
#5743,#5744,#5745,#5746,#5747,#5748,#5749,#5750,#5751,#5752,#5753,#5754,
#5755,#5756,#5757,#5758,#5759,#5760,#5761,#5762,#5763,#5764,#5765,#5766,
#5767,#5768,#5769,#5770,#5771,#5772,#5773,#5774,#5775,#5776,#5777,#5778,
#5779,#5780,#5781,#5782,#5783,#5784,#5785,#5786,#5787,#5788,#5789,#5790,
#5791,#5792,#5793,#5794,#5795,#5796,#5797,#5798));
#1547=EDGE_LOOP('',(#5799,#5800,#5801,#5802));
#1548=EDGE_LOOP('',(#5803,#5804,#5805,#5806));
#1549=EDGE_LOOP('',(#5807,#5808,#5809,#5810));
#1550=EDGE_LOOP('',(#5811,#5812,#5813,#5814));
#1551=EDGE_LOOP('',(#5815,#5816,#5817,#5818));
#1552=EDGE_LOOP('',(#5819,#5820,#5821,#5822));
#1553=EDGE_LOOP('',(#5823,#5824,#5825,#5826));
#1554=EDGE_LOOP('',(#5827,#5828,#5829,#5830,#5831,#5832));
#1555=EDGE_LOOP('',(#5833));
#1556=EDGE_LOOP('',(#5834,#5835,#5836,#5837));
#1557=EDGE_LOOP('',(#5838,#5839,#5840,#5841));
#1558=EDGE_LOOP('',(#5842));
#1559=EDGE_LOOP('',(#5843,#5844,#5845,#5846,#5847,#5848));
#1560=EDGE_LOOP('',(#5849));
#1561=EDGE_LOOP('',(#5850,#5851,#5852));
#1562=EDGE_LOOP('',(#5853,#5854,#5855,#5856,#5857));
#1563=EDGE_LOOP('',(#5858,#5859,#5860,#5861));
#1564=EDGE_LOOP('',(#5862,#5863,#5864,#5865));
#1565=EDGE_LOOP('',(#5866,#5867,#5868,#5869));
#1566=EDGE_LOOP('',(#5870,#5871,#5872,#5873));
#1567=EDGE_LOOP('',(#5874,#5875,#5876,#5877));
#1568=EDGE_LOOP('',(#5878,#5879,#5880,#5881));
#1569=EDGE_LOOP('',(#5882,#5883,#5884,#5885));
#1570=EDGE_LOOP('',(#5886,#5887,#5888,#5889));
#1571=EDGE_LOOP('',(#5890,#5891,#5892,#5893));
#1572=EDGE_LOOP('',(#5894,#5895,#5896,#5897,#5898,#5899,#5900,#5901,#5902,
#5903,#5904,#5905,#5906,#5907));
#1573=EDGE_LOOP('',(#5908,#5909,#5910,#5911,#5912,#5913,#5914,#5915,#5916,
#5917,#5918,#5919,#5920));
#1574=EDGE_LOOP('',(#5921,#5922,#5923,#5924,#5925,#5926));
#1575=EDGE_LOOP('',(#5927,#5928,#5929,#5930));
#1576=EDGE_LOOP('',(#5931,#5932,#5933,#5934));
#1577=EDGE_LOOP('',(#5935,#5936,#5937,#5938));
#1578=EDGE_LOOP('',(#5939,#5940,#5941,#5942));
#1579=EDGE_LOOP('',(#5943,#5944,#5945,#5946));
#1580=EDGE_LOOP('',(#5947,#5948,#5949,#5950));
#1581=EDGE_LOOP('',(#5951,#5952,#5953,#5954));
#1582=EDGE_LOOP('',(#5955,#5956,#5957,#5958));
#1583=EDGE_LOOP('',(#5959,#5960,#5961,#5962,#5963,#5964));
#1584=EDGE_LOOP('',(#5965,#5966,#5967,#5968,#5969));
#1585=EDGE_LOOP('',(#5970,#5971,#5972,#5973));
#1586=EDGE_LOOP('',(#5974,#5975,#5976,#5977));
#1587=EDGE_LOOP('',(#5978));
#1588=EDGE_LOOP('',(#5979));
#1589=EDGE_LOOP('',(#5980));
#1590=EDGE_LOOP('',(#5981));
#1591=LINE('',#8466,#1995);
#1592=LINE('',#8472,#1996);
#1593=LINE('',#8478,#1997);
#1594=LINE('',#8483,#1998);
#1595=LINE('',#8485,#1999);
#1596=LINE('',#8486,#2000);
#1597=LINE('',#8490,#2001);
#1598=LINE('',#8495,#2002);
#1599=LINE('',#8496,#2003);
#1600=LINE('',#8500,#2004);
#1601=LINE('',#8501,#2005);
#1602=LINE('',#8502,#2006);
#1603=LINE('',#8506,#2007);
#1604=LINE('',#8508,#2008);
#1605=LINE('',#8510,#2009);
#1606=LINE('',#8511,#2010);
#1607=LINE('',#8517,#2011);
#1608=LINE('',#8523,#2012);
#1609=LINE('',#8524,#2013);
#1610=LINE('',#8527,#2014);
#1611=LINE('',#8529,#2015);
#1612=LINE('',#8531,#2016);
#1613=LINE('',#8532,#2017);
#1614=LINE('',#8535,#2018);
#1615=LINE('',#8537,#2019);
#1616=LINE('',#8538,#2020);
#1617=LINE('',#8542,#2021);
#1618=LINE('',#8543,#2022);
#1619=LINE('',#8544,#2023);
#1620=LINE('',#8548,#2024);
#1621=LINE('',#8549,#2025);
#1622=LINE('',#8550,#2026);
#1623=LINE('',#8555,#2027);
#1624=LINE('',#8561,#2028);
#1625=LINE('',#8565,#2029);
#1626=LINE('',#8569,#2030);
#1627=LINE('',#8571,#2031);
#1628=LINE('',#8573,#2032);
#1629=LINE('',#8575,#2033);
#1630=LINE('',#8577,#2034);
#1631=LINE('',#8581,#2035);
#1632=LINE('',#8582,#2036);
#1633=LINE('',#8596,#2037);
#1634=LINE('',#8599,#2038);
#1635=LINE('',#8601,#2039);
#1636=LINE('',#8605,#2040);
#1637=LINE('',#8607,#2041);
#1638=LINE('',#8609,#2042);
#1639=LINE('',#8611,#2043);
#1640=LINE('',#8613,#2044);
#1641=LINE('',#8616,#2045);
#1642=LINE('',#8620,#2046);
#1643=LINE('',#8621,#2047);
#1644=LINE('',#8623,#2048);
#1645=LINE('',#8624,#2049);
#1646=LINE('',#8626,#2050);
#1647=LINE('',#8628,#2051);
#1648=LINE('',#8631,#2052);
#1649=LINE('',#8634,#2053);
#1650=LINE('',#8636,#2054);
#1651=LINE('',#8643,#2055);
#1652=LINE('',#8654,#2056);
#1653=LINE('',#8662,#2057);
#1654=LINE('',#8666,#2058);
#1655=LINE('',#8672,#2059);
#1656=LINE('',#8674,#2060);
#1657=LINE('',#8676,#2061);
#1658=LINE('',#8677,#2062);
#1659=LINE('',#8681,#2063);
#1660=LINE('',#8683,#2064);
#1661=LINE('',#8685,#2065);
#1662=LINE('',#8686,#2066);
#1663=LINE('',#8701,#2067);
#1664=LINE('',#8707,#2068);
#1665=LINE('',#8713,#2069);
#1666=LINE('',#8719,#2070);
#1667=LINE('',#8725,#2071);
#1668=LINE('',#8734,#2072);
#1669=LINE('',#8741,#2073);
#1670=LINE('',#8745,#2074);
#1671=LINE('',#8750,#2075);
#1672=LINE('',#8752,#2076);
#1673=LINE('',#8754,#2077);
#1674=LINE('',#8755,#2078);
#1675=LINE('',#8759,#2079);
#1676=LINE('',#8761,#2080);
#1677=LINE('',#8763,#2081);
#1678=LINE('',#8764,#2082);
#1679=LINE('',#8768,#2083);
#1680=LINE('',#8770,#2084);
#1681=LINE('',#8772,#2085);
#1682=LINE('',#8773,#2086);
#1683=LINE('',#8777,#2087);
#1684=LINE('',#8779,#2088);
#1685=LINE('',#8781,#2089);
#1686=LINE('',#8782,#2090);
#1687=LINE('',#8786,#2091);
#1688=LINE('',#8788,#2092);
#1689=LINE('',#8790,#2093);
#1690=LINE('',#8791,#2094);
#1691=LINE('',#8795,#2095);
#1692=LINE('',#8797,#2096);
#1693=LINE('',#8799,#2097);
#1694=LINE('',#8800,#2098);
#1695=LINE('',#8804,#2099);
#1696=LINE('',#8806,#2100);
#1697=LINE('',#8808,#2101);
#1698=LINE('',#8809,#2102);
#1699=LINE('',#8817,#2103);
#1700=LINE('',#8818,#2104);
#1701=LINE('',#8820,#2105);
#1702=LINE('',#8821,#2106);
#1703=LINE('',#8823,#2107);
#1704=LINE('',#8824,#2108);
#1705=LINE('',#8827,#2109);
#1706=LINE('',#8829,#2110);
#1707=LINE('',#8830,#2111);
#1708=LINE('',#8833,#2112);
#1709=LINE('',#8835,#2113);
#1710=LINE('',#8836,#2114);
#1711=LINE('',#8840,#2115);
#1712=LINE('',#8878,#2116);
#1713=LINE('',#8916,#2117);
#1714=LINE('',#8954,#2118);
#1715=LINE('',#8991,#2119);
#1716=LINE('',#8994,#2120);
#1717=LINE('',#9032,#2121);
#1718=LINE('',#9069,#2122);
#1719=LINE('',#9072,#2123);
#1720=LINE('',#9110,#2124);
#1721=LINE('',#9147,#2125);
#1722=LINE('',#9150,#2126);
#1723=LINE('',#9157,#2127);
#1724=LINE('',#9163,#2128);
#1725=LINE('',#9180,#2129);
#1726=LINE('',#9189,#2130);
#1727=LINE('',#9195,#2131);
#1728=LINE('',#9230,#2132);
#1729=LINE('',#9301,#2133);
#1730=LINE('',#9371,#2134);
#1731=LINE('',#9406,#2135);
#1732=LINE('',#9412,#2136);
#1733=LINE('',#9421,#2137);
#1734=LINE('',#9455,#2138);
#1735=LINE('',#9487,#2139);
#1736=LINE('',#9491,#2140);
#1737=LINE('',#9495,#2141);
#1738=LINE('',#9541,#2142);
#1739=LINE('',#9676,#2143);
#1740=LINE('',#9780,#2144);
#1741=LINE('',#9943,#2145);
#1742=LINE('',#10106,#2146);
#1743=LINE('',#10195,#2147);
#1744=LINE('',#10283,#2148);
#1745=LINE('',#10395,#2149);
#1746=LINE('',#10396,#2150);
#1747=LINE('',#10433,#2151);
#1748=LINE('',#10434,#2152);
#1749=LINE('',#10636,#2153);
#1750=LINE('',#10642,#2154);
#1751=LINE('',#10648,#2155);
#1752=LINE('',#10654,#2156);
#1753=LINE('',#10659,#2157);
#1754=LINE('',#10661,#2158);
#1755=LINE('',#10663,#2159);
#1756=LINE('',#10664,#2160);
#1757=LINE('',#10667,#2161);
#1758=LINE('',#10669,#2162);
#1759=LINE('',#10670,#2163);
#1760=LINE('',#10673,#2164);
#1761=LINE('',#10675,#2165);
#1762=LINE('',#10676,#2166);
#1763=LINE('',#10679,#2167);
#1764=LINE('',#10681,#2168);
#1765=LINE('',#10682,#2169);
#1766=LINE('',#10685,#2170);
#1767=LINE('',#10687,#2171);
#1768=LINE('',#10688,#2172);
#1769=LINE('',#10690,#2173);
#1770=LINE('',#10691,#2174);
#1771=LINE('',#10698,#2175);
#1772=LINE('',#10700,#2176);
#1773=LINE('',#10702,#2177);
#1774=LINE('',#10703,#2178);
#1775=LINE('',#10706,#2179);
#1776=LINE('',#10708,#2180);
#1777=LINE('',#10709,#2181);
#1778=LINE('',#10712,#2182);
#1779=LINE('',#10714,#2183);
#1780=LINE('',#10715,#2184);
#1781=LINE('',#10718,#2185);
#1782=LINE('',#10720,#2186);
#1783=LINE('',#10721,#2187);
#1784=LINE('',#10724,#2188);
#1785=LINE('',#10726,#2189);
#1786=LINE('',#10727,#2190);
#1787=LINE('',#10729,#2191);
#1788=LINE('',#10730,#2192);
#1789=LINE('',#10736,#2193);
#1790=LINE('',#10740,#2194);
#1791=LINE('',#10745,#2195);
#1792=LINE('',#10747,#2196);
#1793=LINE('',#10749,#2197);
#1794=LINE('',#10750,#2198);
#1795=LINE('',#10754,#2199);
#1796=LINE('',#10756,#2200);
#1797=LINE('',#10758,#2201);
#1798=LINE('',#10759,#2202);
#1799=LINE('',#10763,#2203);
#1800=LINE('',#10765,#2204);
#1801=LINE('',#10767,#2205);
#1802=LINE('',#10768,#2206);
#1803=LINE('',#10772,#2207);
#1804=LINE('',#10774,#2208);
#1805=LINE('',#10776,#2209);
#1806=LINE('',#10777,#2210);
#1807=LINE('',#10781,#2211);
#1808=LINE('',#10783,#2212);
#1809=LINE('',#10785,#2213);
#1810=LINE('',#10786,#2214);
#1811=LINE('',#10790,#2215);
#1812=LINE('',#10792,#2216);
#1813=LINE('',#10794,#2217);
#1814=LINE('',#10795,#2218);
#1815=LINE('',#10799,#2219);
#1816=LINE('',#10801,#2220);
#1817=LINE('',#10803,#2221);
#1818=LINE('',#10804,#2222);
#1819=LINE('',#10812,#2223);
#1820=LINE('',#10813,#2224);
#1821=LINE('',#10815,#2225);
#1822=LINE('',#10816,#2226);
#1823=LINE('',#10818,#2227);
#1824=LINE('',#10819,#2228);
#1825=LINE('',#10822,#2229);
#1826=LINE('',#10824,#2230);
#1827=LINE('',#10825,#2231);
#1828=LINE('',#10828,#2232);
#1829=LINE('',#10830,#2233);
#1830=LINE('',#10831,#2234);
#1831=LINE('',#10835,#2235);
#1832=LINE('',#10873,#2236);
#1833=LINE('',#10911,#2237);
#1834=LINE('',#10949,#2238);
#1835=LINE('',#10986,#2239);
#1836=LINE('',#10989,#2240);
#1837=LINE('',#11027,#2241);
#1838=LINE('',#11064,#2242);
#1839=LINE('',#11067,#2243);
#1840=LINE('',#11105,#2244);
#1841=LINE('',#11142,#2245);
#1842=LINE('',#11145,#2246);
#1843=LINE('',#11152,#2247);
#1844=LINE('',#11158,#2248);
#1845=LINE('',#11175,#2249);
#1846=LINE('',#11184,#2250);
#1847=LINE('',#11190,#2251);
#1848=LINE('',#11225,#2252);
#1849=LINE('',#11296,#2253);
#1850=LINE('',#11366,#2254);
#1851=LINE('',#11401,#2255);
#1852=LINE('',#11407,#2256);
#1853=LINE('',#11416,#2257);
#1854=LINE('',#11450,#2258);
#1855=LINE('',#11482,#2259);
#1856=LINE('',#11486,#2260);
#1857=LINE('',#11490,#2261);
#1858=LINE('',#11536,#2262);
#1859=LINE('',#11671,#2263);
#1860=LINE('',#11775,#2264);
#1861=LINE('',#11938,#2265);
#1862=LINE('',#12101,#2266);
#1863=LINE('',#12190,#2267);
#1864=LINE('',#12278,#2268);
#1865=LINE('',#12390,#2269);
#1866=LINE('',#12391,#2270);
#1867=LINE('',#12428,#2271);
#1868=LINE('',#12429,#2272);
#1869=LINE('',#12631,#2273);
#1870=LINE('',#12637,#2274);
#1871=LINE('',#12647,#2275);
#1872=LINE('',#12657,#2276);
#1873=LINE('',#12667,#2277);
#1874=LINE('',#12677,#2278);
#1875=LINE('',#12681,#2279);
#1876=LINE('',#12685,#2280);
#1877=LINE('',#12689,#2281);
#1878=LINE('',#12693,#2282);
#1879=LINE('',#12740,#2283);
#1880=LINE('',#12741,#2284);
#1881=LINE('',#12867,#2285);
#1882=LINE('',#12868,#2286);
#1883=LINE('',#12956,#2287);
#1884=LINE('',#13096,#2288);
#1885=LINE('',#13225,#2289);
#1886=LINE('',#13249,#2290);
#1887=LINE('',#13297,#2291);
#1888=LINE('',#13345,#2292);
#1889=LINE('',#13396,#2293);
#1890=LINE('',#13444,#2294);
#1891=LINE('',#13492,#2295);
#1892=LINE('',#13540,#2296);
#1893=LINE('',#13594,#2297);
#1894=LINE('',#13642,#2298);
#1895=LINE('',#13690,#2299);
#1896=LINE('',#13744,#2300);
#1897=LINE('',#13792,#2301);
#1898=LINE('',#13840,#2302);
#1899=LINE('',#13888,#2303);
#1900=LINE('',#13942,#2304);
#1901=LINE('',#13990,#2305);
#1902=LINE('',#14038,#2306);
#1903=LINE('',#14092,#2307);
#1904=LINE('',#14140,#2308);
#1905=LINE('',#14188,#2309);
#1906=LINE('',#14242,#2310);
#1907=LINE('',#14290,#2311);
#1908=LINE('',#14338,#2312);
#1909=LINE('',#14386,#2313);
#1910=LINE('',#14440,#2314);
#1911=LINE('',#14488,#2315);
#1912=LINE('',#14536,#2316);
#1913=LINE('',#14590,#2317);
#1914=LINE('',#14638,#2318);
#1915=LINE('',#14686,#2319);
#1916=LINE('',#14712,#2320);
#1917=LINE('',#14736,#2321);
#1918=LINE('',#14760,#2322);
#1919=LINE('',#14785,#2323);
#1920=LINE('',#14810,#2324);
#1921=LINE('',#14834,#2325);
#1922=LINE('',#14859,#2326);
#1923=LINE('',#14884,#2327);
#1924=LINE('',#14908,#2328);
#1925=LINE('',#14932,#2329);
#1926=LINE('',#14957,#2330);
#1927=LINE('',#14982,#2331);
#1928=LINE('',#15006,#2332);
#1929=LINE('',#15031,#2333);
#1930=LINE('',#15056,#2334);
#1931=LINE('',#15080,#2335);
#1932=LINE('',#15105,#2336);
#1933=LINE('',#15130,#2337);
#1934=LINE('',#15154,#2338);
#1935=LINE('',#15178,#2339);
#1936=LINE('',#15203,#2340);
#1937=LINE('',#15228,#2341);
#1938=LINE('',#15252,#2342);
#1939=LINE('',#15277,#2343);
#1940=LINE('',#15302,#2344);
#1941=LINE('',#15326,#2345);
#1942=LINE('',#15351,#2346);
#1943=LINE('',#15375,#2347);
#1944=LINE('',#15400,#2348);
#1945=LINE('',#15601,#2349);
#1946=LINE('',#17346,#2350);
#1947=LINE('',#17348,#2351);
#1948=LINE('',#17350,#2352);
#1949=LINE('',#17351,#2353);
#1950=LINE('',#17354,#2354);
#1951=LINE('',#17356,#2355);
#1952=LINE('',#17357,#2356);
#1953=LINE('',#17360,#2357);
#1954=LINE('',#17362,#2358);
#1955=LINE('',#17363,#2359);
#1956=LINE('',#17366,#2360);
#1957=LINE('',#17368,#2361);
#1958=LINE('',#17369,#2362);
#1959=LINE('',#17372,#2363);
#1960=LINE('',#17374,#2364);
#1961=LINE('',#17375,#2365);
#1962=LINE('',#17377,#2366);
#1963=LINE('',#17378,#2367);
#1964=LINE('',#17385,#2368);
#1965=LINE('',#17393,#2369);
#1966=LINE('',#17406,#2370);
#1967=LINE('',#17453,#2371);
#1968=LINE('',#17507,#2372);
#1969=LINE('',#17555,#2373);
#1970=LINE('',#17594,#2374);
#1971=LINE('',#17615,#2375);
#1972=LINE('',#17640,#2376);
#1973=LINE('',#17665,#2377);
#1974=LINE('',#17690,#2378);
#1975=LINE('',#18263,#2379);
#1976=LINE('',#18265,#2380);
#1977=LINE('',#18267,#2381);
#1978=LINE('',#18269,#2382);
#1979=LINE('',#18271,#2383);
#1980=LINE('',#18272,#2384);
#1981=LINE('',#18277,#2385);
#1982=LINE('',#18278,#2386);
#1983=LINE('',#18279,#2387);
#1984=LINE('',#18282,#2388);
#1985=LINE('',#18283,#2389);
#1986=LINE('',#18286,#2390);
#1987=LINE('',#18287,#2391);
#1988=LINE('',#18290,#2392);
#1989=LINE('',#18291,#2393);
#1990=LINE('',#18294,#2394);
#1991=LINE('',#18295,#2395);
#1992=LINE('',#18297,#2396);
#1993=LINE('',#18312,#2397);
#1994=LINE('',#18318,#2398);
#1995=VECTOR('',#7090,0.17);
#1996=VECTOR('',#7097,0.17);
#1997=VECTOR('',#7104,0.41);
#1998=VECTOR('',#7109,1.);
#1999=VECTOR('',#7110,1.);
#2000=VECTOR('',#7111,1.);
#2001=VECTOR('',#7114,1.);
#2002=VECTOR('',#7121,1.);
#2003=VECTOR('',#7122,1.);
#2004=VECTOR('',#7125,1.);
#2005=VECTOR('',#7126,1.);
#2006=VECTOR('',#7127,1.);
#2007=VECTOR('',#7130,1.);
#2008=VECTOR('',#7131,1.);
#2009=VECTOR('',#7132,1.);
#2010=VECTOR('',#7133,1.);
#2011=VECTOR('',#7140,1.);
#2012=VECTOR('',#7149,1.);
#2013=VECTOR('',#7150,1.);
#2014=VECTOR('',#7153,1.);
#2015=VECTOR('',#7154,1.);
#2016=VECTOR('',#7155,1.);
#2017=VECTOR('',#7156,1.);
#2018=VECTOR('',#7159,1.);
#2019=VECTOR('',#7160,1.);
#2020=VECTOR('',#7161,1.);
#2021=VECTOR('',#7164,1.);
#2022=VECTOR('',#7165,1.);
#2023=VECTOR('',#7166,1.);
#2024=VECTOR('',#7169,1.);
#2025=VECTOR('',#7170,1.);
#2026=VECTOR('',#7171,1.);
#2027=VECTOR('',#7176,1.);
#2028=VECTOR('',#7183,1.);
#2029=VECTOR('',#7188,1.);
#2030=VECTOR('',#7191,1.);
#2031=VECTOR('',#7192,1.);
#2032=VECTOR('',#7193,1.);
#2033=VECTOR('',#7194,1.);
#2034=VECTOR('',#7195,1.);
#2035=VECTOR('',#7198,1.);
#2036=VECTOR('',#7199,1.);
#2037=VECTOR('',#7216,1.1);
#2038=VECTOR('',#7219,1.);
#2039=VECTOR('',#7220,1.);
#2040=VECTOR('',#7223,1.);
#2041=VECTOR('',#7224,1.);
#2042=VECTOR('',#7225,1.);
#2043=VECTOR('',#7226,1.);
#2044=VECTOR('',#7227,1.);
#2045=VECTOR('',#7230,1.);
#2046=VECTOR('',#7237,1.);
#2047=VECTOR('',#7238,1.);
#2048=VECTOR('',#7241,1.);
#2049=VECTOR('',#7242,1.);
#2050=VECTOR('',#7245,1.);
#2051=VECTOR('',#7248,1.);
#2052=VECTOR('',#7253,1.);
#2053=VECTOR('',#7258,1.);
#2054=VECTOR('',#7261,1.);
#2055=VECTOR('',#7270,0.3);
#2056=VECTOR('',#7285,0.4);
#2057=VECTOR('',#7294,0.6);
#2058=VECTOR('',#7301,0.4);
#2059=VECTOR('',#7308,1.);
#2060=VECTOR('',#7309,1.);
#2061=VECTOR('',#7310,1.);
#2062=VECTOR('',#7311,1.);
#2063=VECTOR('',#7314,1.);
#2064=VECTOR('',#7315,1.);
#2065=VECTOR('',#7316,1.);
#2066=VECTOR('',#7317,1.);
#2067=VECTOR('',#7342,0.15);
#2068=VECTOR('',#7349,0.15);
#2069=VECTOR('',#7356,0.15);
#2070=VECTOR('',#7363,0.15);
#2071=VECTOR('',#7370,0.3);
#2072=VECTOR('',#7381,0.3);
#2073=VECTOR('',#7390,0.17);
#2074=VECTOR('',#7395,0.17);
#2075=VECTOR('',#7400,1.);
#2076=VECTOR('',#7401,1.);
#2077=VECTOR('',#7402,1.);
#2078=VECTOR('',#7403,1.);
#2079=VECTOR('',#7406,1.);
#2080=VECTOR('',#7407,1.);
#2081=VECTOR('',#7408,1.);
#2082=VECTOR('',#7409,1.);
#2083=VECTOR('',#7412,1.);
#2084=VECTOR('',#7413,1.);
#2085=VECTOR('',#7414,1.);
#2086=VECTOR('',#7415,1.);
#2087=VECTOR('',#7418,1.);
#2088=VECTOR('',#7419,1.);
#2089=VECTOR('',#7420,1.);
#2090=VECTOR('',#7421,1.);
#2091=VECTOR('',#7424,1.);
#2092=VECTOR('',#7425,1.);
#2093=VECTOR('',#7426,1.);
#2094=VECTOR('',#7427,1.);
#2095=VECTOR('',#7430,1.);
#2096=VECTOR('',#7431,1.);
#2097=VECTOR('',#7432,1.);
#2098=VECTOR('',#7433,1.);
#2099=VECTOR('',#7436,1.);
#2100=VECTOR('',#7437,1.);
#2101=VECTOR('',#7438,1.);
#2102=VECTOR('',#7439,1.);
#2103=VECTOR('',#7450,1.);
#2104=VECTOR('',#7451,1.);
#2105=VECTOR('',#7454,1.);
#2106=VECTOR('',#7455,1.);
#2107=VECTOR('',#7458,1.);
#2108=VECTOR('',#7459,1.);
#2109=VECTOR('',#7462,1.);
#2110=VECTOR('',#7463,1.);
#2111=VECTOR('',#7464,1.);
#2112=VECTOR('',#7467,1.);
#2113=VECTOR('',#7468,1.);
#2114=VECTOR('',#7469,1.);
#2115=VECTOR('',#7472,1.);
#2116=VECTOR('',#7473,1.);
#2117=VECTOR('',#7476,1.);
#2118=VECTOR('',#7477,1.);
#2119=VECTOR('',#7478,1.);
#2120=VECTOR('',#7481,1.);
#2121=VECTOR('',#7482,1.);
#2122=VECTOR('',#7483,1.);
#2123=VECTOR('',#7486,1.);
#2124=VECTOR('',#7487,1.);
#2125=VECTOR('',#7488,1.);
#2126=VECTOR('',#7491,1.);
#2127=VECTOR('',#7492,1.);
#2128=VECTOR('',#7493,1.);
#2129=VECTOR('',#7496,1.);
#2130=VECTOR('',#7497,1.);
#2131=VECTOR('',#7498,1.);
#2132=VECTOR('',#7499,1.);
#2133=VECTOR('',#7500,1.);
#2134=VECTOR('',#7501,1.);
#2135=VECTOR('',#7502,1.);
#2136=VECTOR('',#7503,1.);
#2137=VECTOR('',#7504,1.);
#2138=VECTOR('',#7505,1.);
#2139=VECTOR('',#7506,1.);
#2140=VECTOR('',#7511,0.4);
#2141=VECTOR('',#7516,0.4);
#2142=VECTOR('',#7519,1.);
#2143=VECTOR('',#7526,1.);
#2144=VECTOR('',#7529,1.);
#2145=VECTOR('',#7534,1.);
#2146=VECTOR('',#7539,1.);
#2147=VECTOR('',#7544,1.);
#2148=VECTOR('',#7577,1.);
#2149=VECTOR('',#7606,1.);
#2150=VECTOR('',#7607,1.);
#2151=VECTOR('',#7618,1.);
#2152=VECTOR('',#7619,1.);
#2153=VECTOR('',#7632,0.15);
#2154=VECTOR('',#7639,0.15);
#2155=VECTOR('',#7646,0.15);
#2156=VECTOR('',#7653,0.15);
#2157=VECTOR('',#7658,1.);
#2158=VECTOR('',#7659,1.);
#2159=VECTOR('',#7660,1.);
#2160=VECTOR('',#7661,1.);
#2161=VECTOR('',#7664,1.);
#2162=VECTOR('',#7665,1.);
#2163=VECTOR('',#7666,1.);
#2164=VECTOR('',#7669,1.);
#2165=VECTOR('',#7670,1.);
#2166=VECTOR('',#7671,1.);
#2167=VECTOR('',#7674,1.);
#2168=VECTOR('',#7675,1.);
#2169=VECTOR('',#7676,1.);
#2170=VECTOR('',#7679,1.);
#2171=VECTOR('',#7680,1.);
#2172=VECTOR('',#7681,1.);
#2173=VECTOR('',#7684,1.);
#2174=VECTOR('',#7685,1.);
#2175=VECTOR('',#7692,1.);
#2176=VECTOR('',#7693,1.);
#2177=VECTOR('',#7694,1.);
#2178=VECTOR('',#7695,1.);
#2179=VECTOR('',#7698,1.);
#2180=VECTOR('',#7699,1.);
#2181=VECTOR('',#7700,1.);
#2182=VECTOR('',#7703,1.);
#2183=VECTOR('',#7704,1.);
#2184=VECTOR('',#7705,1.);
#2185=VECTOR('',#7708,1.);
#2186=VECTOR('',#7709,1.);
#2187=VECTOR('',#7710,1.);
#2188=VECTOR('',#7713,1.);
#2189=VECTOR('',#7714,1.);
#2190=VECTOR('',#7715,1.);
#2191=VECTOR('',#7718,1.);
#2192=VECTOR('',#7719,1.);
#2193=VECTOR('',#7726,0.17);
#2194=VECTOR('',#7731,0.17);
#2195=VECTOR('',#7736,1.);
#2196=VECTOR('',#7737,1.);
#2197=VECTOR('',#7738,1.);
#2198=VECTOR('',#7739,1.);
#2199=VECTOR('',#7742,1.);
#2200=VECTOR('',#7743,1.);
#2201=VECTOR('',#7744,1.);
#2202=VECTOR('',#7745,1.);
#2203=VECTOR('',#7748,1.);
#2204=VECTOR('',#7749,1.);
#2205=VECTOR('',#7750,1.);
#2206=VECTOR('',#7751,1.);
#2207=VECTOR('',#7754,1.);
#2208=VECTOR('',#7755,1.);
#2209=VECTOR('',#7756,1.);
#2210=VECTOR('',#7757,1.);
#2211=VECTOR('',#7760,1.);
#2212=VECTOR('',#7761,1.);
#2213=VECTOR('',#7762,1.);
#2214=VECTOR('',#7763,1.);
#2215=VECTOR('',#7766,1.);
#2216=VECTOR('',#7767,1.);
#2217=VECTOR('',#7768,1.);
#2218=VECTOR('',#7769,1.);
#2219=VECTOR('',#7772,1.);
#2220=VECTOR('',#7773,1.);
#2221=VECTOR('',#7774,1.);
#2222=VECTOR('',#7775,1.);
#2223=VECTOR('',#7786,1.);
#2224=VECTOR('',#7787,1.);
#2225=VECTOR('',#7790,1.);
#2226=VECTOR('',#7791,1.);
#2227=VECTOR('',#7794,1.);
#2228=VECTOR('',#7795,1.);
#2229=VECTOR('',#7798,1.);
#2230=VECTOR('',#7799,1.);
#2231=VECTOR('',#7800,1.);
#2232=VECTOR('',#7803,1.);
#2233=VECTOR('',#7804,1.);
#2234=VECTOR('',#7805,1.);
#2235=VECTOR('',#7808,1.);
#2236=VECTOR('',#7809,1.);
#2237=VECTOR('',#7812,1.);
#2238=VECTOR('',#7813,1.);
#2239=VECTOR('',#7814,1.);
#2240=VECTOR('',#7817,1.);
#2241=VECTOR('',#7818,1.);
#2242=VECTOR('',#7819,1.);
#2243=VECTOR('',#7822,1.);
#2244=VECTOR('',#7823,1.);
#2245=VECTOR('',#7824,1.);
#2246=VECTOR('',#7827,1.);
#2247=VECTOR('',#7828,1.);
#2248=VECTOR('',#7829,1.);
#2249=VECTOR('',#7832,1.);
#2250=VECTOR('',#7833,1.);
#2251=VECTOR('',#7834,1.);
#2252=VECTOR('',#7835,1.);
#2253=VECTOR('',#7836,1.);
#2254=VECTOR('',#7837,1.);
#2255=VECTOR('',#7838,1.);
#2256=VECTOR('',#7839,1.);
#2257=VECTOR('',#7840,1.);
#2258=VECTOR('',#7841,1.);
#2259=VECTOR('',#7842,1.);
#2260=VECTOR('',#7847,0.4);
#2261=VECTOR('',#7852,0.4);
#2262=VECTOR('',#7855,1.);
#2263=VECTOR('',#7862,1.);
#2264=VECTOR('',#7865,1.);
#2265=VECTOR('',#7870,1.);
#2266=VECTOR('',#7875,1.);
#2267=VECTOR('',#7880,1.);
#2268=VECTOR('',#7913,1.);
#2269=VECTOR('',#7942,1.);
#2270=VECTOR('',#7943,1.);
#2271=VECTOR('',#7954,1.);
#2272=VECTOR('',#7955,1.);
#2273=VECTOR('',#7968,0.35);
#2274=VECTOR('',#7975,0.35);
#2275=VECTOR('',#7988,0.25);
#2276=VECTOR('',#8001,0.25);
#2277=VECTOR('',#8014,0.25);
#2278=VECTOR('',#8027,0.25);
#2279=VECTOR('',#8032,0.15);
#2280=VECTOR('',#8037,0.15);
#2281=VECTOR('',#8042,0.15);
#2282=VECTOR('',#8047,0.15);
#2283=VECTOR('',#8058,1.);
#2284=VECTOR('',#8059,1.);
#2285=VECTOR('',#8070,1.);
#2286=VECTOR('',#8071,1.);
#2287=VECTOR('',#8076,1.);
#2288=VECTOR('',#8081,1.);
#2289=VECTOR('',#8088,0.15);
#2290=VECTOR('',#8093,0.15);
#2291=VECTOR('',#8096,0.15);
#2292=VECTOR('',#8099,0.15);
#2293=VECTOR('',#8102,0.15);
#2294=VECTOR('',#8105,0.15);
#2295=VECTOR('',#8108,0.15);
#2296=VECTOR('',#8111,0.15);
#2297=VECTOR('',#8114,0.15);
#2298=VECTOR('',#8117,0.15);
#2299=VECTOR('',#8120,0.15);
#2300=VECTOR('',#8123,0.15);
#2301=VECTOR('',#8126,0.15);
#2302=VECTOR('',#8129,0.15);
#2303=VECTOR('',#8132,0.15);
#2304=VECTOR('',#8135,0.15);
#2305=VECTOR('',#8138,0.15);
#2306=VECTOR('',#8141,0.15);
#2307=VECTOR('',#8144,0.15);
#2308=VECTOR('',#8147,0.15);
#2309=VECTOR('',#8150,0.15);
#2310=VECTOR('',#8153,0.15);
#2311=VECTOR('',#8156,0.15);
#2312=VECTOR('',#8159,0.15);
#2313=VECTOR('',#8162,0.15);
#2314=VECTOR('',#8165,0.15);
#2315=VECTOR('',#8168,0.15);
#2316=VECTOR('',#8171,0.15);
#2317=VECTOR('',#8174,0.15);
#2318=VECTOR('',#8177,0.15);
#2319=VECTOR('',#8180,0.117775);
#2320=VECTOR('',#8185,0.117775);
#2321=VECTOR('',#8188,0.117775);
#2322=VECTOR('',#8191,0.117775);
#2323=VECTOR('',#8194,0.117775);
#2324=VECTOR('',#8197,0.117775);
#2325=VECTOR('',#8200,0.117775);
#2326=VECTOR('',#8203,0.117775);
#2327=VECTOR('',#8206,0.117775);
#2328=VECTOR('',#8209,0.117775);
#2329=VECTOR('',#8212,0.117775);
#2330=VECTOR('',#8215,0.117775);
#2331=VECTOR('',#8218,0.117775);
#2332=VECTOR('',#8221,0.117775);
#2333=VECTOR('',#8224,0.117775);
#2334=VECTOR('',#8227,0.117775);
#2335=VECTOR('',#8230,0.117775);
#2336=VECTOR('',#8233,0.117775);
#2337=VECTOR('',#8236,0.117775);
#2338=VECTOR('',#8239,0.117775);
#2339=VECTOR('',#8242,0.117775);
#2340=VECTOR('',#8245,0.117775);
#2341=VECTOR('',#8248,0.117775);
#2342=VECTOR('',#8251,0.117775);
#2343=VECTOR('',#8254,0.117775);
#2344=VECTOR('',#8257,0.117775);
#2345=VECTOR('',#8260,0.117775);
#2346=VECTOR('',#8263,0.117775);
#2347=VECTOR('',#8266,0.117775);
#2348=VECTOR('',#8269,0.117775);
#2349=VECTOR('',#8274,0.1);
#2350=VECTOR('',#8285,1.);
#2351=VECTOR('',#8286,1.);
#2352=VECTOR('',#8287,1.);
#2353=VECTOR('',#8288,1.);
#2354=VECTOR('',#8291,1.);
#2355=VECTOR('',#8292,1.);
#2356=VECTOR('',#8293,1.);
#2357=VECTOR('',#8296,1.);
#2358=VECTOR('',#8297,1.);
#2359=VECTOR('',#8298,1.);
#2360=VECTOR('',#8301,1.);
#2361=VECTOR('',#8302,1.);
#2362=VECTOR('',#8303,1.);
#2363=VECTOR('',#8306,1.);
#2364=VECTOR('',#8307,1.);
#2365=VECTOR('',#8308,1.);
#2366=VECTOR('',#8311,1.);
#2367=VECTOR('',#8312,1.);
#2368=VECTOR('',#8321,0.275);
#2369=VECTOR('',#8332,0.15);
#2370=VECTOR('',#8337,0.15);
#2371=VECTOR('',#8342,0.15);
#2372=VECTOR('',#8345,0.15);
#2373=VECTOR('',#8348,0.15);
#2374=VECTOR('',#8353,0.1543);
#2375=VECTOR('',#8358,0.1543);
#2376=VECTOR('',#8361,0.1543);
#2377=VECTOR('',#8364,0.1543);
#2378=VECTOR('',#8367,0.1543);
#2379=VECTOR('',#8374,1.);
#2380=VECTOR('',#8375,1.);
#2381=VECTOR('',#8376,1.);
#2382=VECTOR('',#8377,1.);
#2383=VECTOR('',#8378,1.);
#2384=VECTOR('',#8379,1.);
#2385=VECTOR('',#8384,1.);
#2386=VECTOR('',#8385,1.);
#2387=VECTOR('',#8386,1.);
#2388=VECTOR('',#8389,1.);
#2389=VECTOR('',#8390,1.);
#2390=VECTOR('',#8393,1.);
#2391=VECTOR('',#8394,1.);
#2392=VECTOR('',#8397,1.);
#2393=VECTOR('',#8398,1.);
#2394=VECTOR('',#8401,1.);
#2395=VECTOR('',#8402,1.);
#2396=VECTOR('',#8405,1.);
#2397=VECTOR('',#8430,0.41);
#2398=VECTOR('',#8437,0.6);
#2399=CIRCLE('',#6598,0.17);
#2400=CIRCLE('',#6599,0.17);
#2401=CIRCLE('',#6601,0.17);
#2402=CIRCLE('',#6602,0.17);
#2403=CIRCLE('',#6604,0.41);
#2404=CIRCLE('',#6605,0.41);
#2405=CIRCLE('',#6608,4.4044765934785);
#2406=CIRCLE('',#6609,4.0044765934785);
#2407=CIRCLE('',#6614,0.2);
#2408=CIRCLE('',#6615,0.2);
#2409=CIRCLE('',#6617,12.0894198846614);
#2410=CIRCLE('',#6618,12.0894198846614);
#2411=CIRCLE('',#6625,1.4);
#2412=CIRCLE('',#6626,1.4);
#2413=CIRCLE('',#6628,1.4);
#2414=CIRCLE('',#6629,1.4);
#2415=CIRCLE('',#6631,1.7);
#2416=CIRCLE('',#6632,1.7);
#2417=CIRCLE('',#6633,1.2);
#2418=CIRCLE('',#6635,1.2);
#2419=CIRCLE('',#6636,0.1);
#2420=CIRCLE('',#6637,1.1);
#2421=CIRCLE('',#6639,1.1);
#2422=CIRCLE('',#6640,1.1);
#2423=CIRCLE('',#6642,1.7);
#2424=CIRCLE('',#6643,1.7);
#2425=CIRCLE('',#6645,0.1);
#2426=CIRCLE('',#6658,0.3);
#2427=CIRCLE('',#6659,0.3);
#2428=CIRCLE('',#6661,0.4);
#2429=CIRCLE('',#6663,0.4);
#2430=CIRCLE('',#6665,0.4);
#2431=CIRCLE('',#6667,0.6);
#2432=CIRCLE('',#6668,0.4);
#2433=CIRCLE('',#6670,0.6);
#2434=CIRCLE('',#6678,0.6);
#2435=CIRCLE('',#6679,0.3);
#2436=CIRCLE('',#6681,0.3);
#2437=CIRCLE('',#6683,0.6);
#2438=CIRCLE('',#6688,0.15);
#2439=CIRCLE('',#6689,0.15);
#2440=CIRCLE('',#6691,0.15);
#2441=CIRCLE('',#6692,0.15);
#2442=CIRCLE('',#6694,0.15);
#2443=CIRCLE('',#6695,0.15);
#2444=CIRCLE('',#6697,0.15);
#2445=CIRCLE('',#6698,0.15);
#2446=CIRCLE('',#6700,0.3);
#2447=CIRCLE('',#6701,0.3);
#2448=CIRCLE('',#6703,0.17);
#2449=CIRCLE('',#6705,0.3);
#2450=CIRCLE('',#6706,0.3);
#2451=CIRCLE('',#6708,0.17);
#2452=CIRCLE('',#6710,0.17);
#2453=CIRCLE('',#6712,0.17);
#2454=CIRCLE('',#6721,0.4);
#2455=CIRCLE('',#6723,0.4);
#2456=CIRCLE('',#6736,0.4);
#2457=CIRCLE('',#6738,0.4);
#2458=CIRCLE('',#6740,0.1);
#2459=CIRCLE('',#6748,0.0999999999999994);
#2460=CIRCLE('',#6750,0.0999999999999999);
#2461=CIRCLE('',#6752,0.1);
#2462=CIRCLE('',#6753,0.1);
#2463=CIRCLE('',#6755,0.100000000000001);
#2464=CIRCLE('',#6756,0.100000000000001);
#2465=CIRCLE('',#6757,0.100000000000002);
#2466=CIRCLE('',#6759,0.0999999999999995);
#2467=CIRCLE('',#6760,0.0999999999999991);
#2468=CIRCLE('',#6763,0.100000000000001);
#2469=CIRCLE('',#6764,0.1);
#2470=CIRCLE('',#6768,0.3);
#2471=CIRCLE('',#6769,0.3);
#2472=CIRCLE('',#6770,0.3);
#2473=CIRCLE('',#6772,0.3);
#2474=CIRCLE('',#6773,0.300000000000002);
#2475=CIRCLE('',#6774,0.3);
#2476=CIRCLE('',#6776,0.3);
#2477=CIRCLE('',#6777,0.299999999999999);
#2478=CIRCLE('',#6778,0.3);
#2479=CIRCLE('',#6781,0.300000000000001);
#2480=CIRCLE('',#6782,0.3);
#2481=CIRCLE('',#6783,0.3);
#2482=CIRCLE('',#6790,0.15);
#2483=CIRCLE('',#6791,0.15);
#2484=CIRCLE('',#6793,0.15);
#2485=CIRCLE('',#6794,0.15);
#2486=CIRCLE('',#6796,0.15);
#2487=CIRCLE('',#6797,0.15);
#2488=CIRCLE('',#6799,0.15);
#2489=CIRCLE('',#6800,0.15);
#2490=CIRCLE('',#6808,0.17);
#2491=CIRCLE('',#6816,0.17);
#2492=CIRCLE('',#6818,0.17);
#2493=CIRCLE('',#6820,0.17);
#2494=CIRCLE('',#6829,0.4);
#2495=CIRCLE('',#6831,0.4);
#2496=CIRCLE('',#6844,0.4);
#2497=CIRCLE('',#6846,0.4);
#2498=CIRCLE('',#6848,0.1);
#2499=CIRCLE('',#6856,0.0999999999999994);
#2500=CIRCLE('',#6858,0.0999999999999999);
#2501=CIRCLE('',#6860,0.1);
#2502=CIRCLE('',#6861,0.1);
#2503=CIRCLE('',#6863,0.100000000000001);
#2504=CIRCLE('',#6864,0.100000000000001);
#2505=CIRCLE('',#6865,0.100000000000002);
#2506=CIRCLE('',#6867,0.0999999999999995);
#2507=CIRCLE('',#6868,0.0999999999999991);
#2508=CIRCLE('',#6871,0.100000000000001);
#2509=CIRCLE('',#6872,0.1);
#2510=CIRCLE('',#6876,0.3);
#2511=CIRCLE('',#6877,0.3);
#2512=CIRCLE('',#6878,0.3);
#2513=CIRCLE('',#6880,0.3);
#2514=CIRCLE('',#6881,0.300000000000002);
#2515=CIRCLE('',#6882,0.3);
#2516=CIRCLE('',#6884,0.3);
#2517=CIRCLE('',#6885,0.299999999999999);
#2518=CIRCLE('',#6886,0.3);
#2519=CIRCLE('',#6889,0.300000000000001);
#2520=CIRCLE('',#6890,0.3);
#2521=CIRCLE('',#6891,0.3);
#2522=CIRCLE('',#6898,0.35);
#2523=CIRCLE('',#6899,0.35);
#2524=CIRCLE('',#6901,0.35);
#2525=CIRCLE('',#6902,0.35);
#2526=CIRCLE('',#6904,0.25);
#2527=CIRCLE('',#6905,0.15);
#2528=CIRCLE('',#6907,0.25);
#2529=CIRCLE('',#6910,0.25);
#2530=CIRCLE('',#6911,0.15);
#2531=CIRCLE('',#6913,0.25);
#2532=CIRCLE('',#6916,0.25);
#2533=CIRCLE('',#6917,0.15);
#2534=CIRCLE('',#6919,0.25);
#2535=CIRCLE('',#6922,0.25);
#2536=CIRCLE('',#6923,0.15);
#2537=CIRCLE('',#6925,0.25);
#2538=CIRCLE('',#6928,0.15);
#2539=CIRCLE('',#6930,0.15);
#2540=CIRCLE('',#6932,0.15);
#2541=CIRCLE('',#6934,0.15);
#2542=CIRCLE('',#6935,0.0800000000000001);
#2543=CIRCLE('',#6936,0.0799999999999999);
#2544=CIRCLE('',#6938,0.0800000000000001);
#2545=CIRCLE('',#6939,0.0799999999999998);
#2546=CIRCLE('',#6940,0.0800000000000001);
#2547=CIRCLE('',#6941,0.0800000000000001);
#2548=CIRCLE('',#6943,0.0800000000000001);
#2549=CIRCLE('',#6944,0.0799999999999998);
#2550=CIRCLE('',#6951,0.14635);
#2551=CIRCLE('',#6982,0.117775);
#2552=CIRCLE('',#7013,0.14635);
#2553=CIRCLE('',#7014,0.05);
#2554=CIRCLE('',#7016,0.117775);
#2555=CIRCLE('',#7026,0.275);
#2556=CIRCLE('',#7028,0.275);
#2557=CIRCLE('',#7033,0.12645);
#2558=CIRCLE('',#7035,0.12645);
#2559=CIRCLE('',#7039,0.12645);
#2560=CIRCLE('',#7041,0.1543);
#2561=CIRCLE('',#7046,0.1543);
#2562=CIRCLE('',#7067,0.41);
#2563=CIRCLE('',#7068,0.41);
#2564=CIRCLE('',#7070,0.6);
#2565=CIRCLE('',#7071,0.6);
#2566=VERTEX_POINT('',#8463);
#2567=VERTEX_POINT('',#8465);
#2568=VERTEX_POINT('',#8469);
#2569=VERTEX_POINT('',#8471);
#2570=VERTEX_POINT('',#8475);
#2571=VERTEX_POINT('',#8477);
#2572=VERTEX_POINT('',#8481);
#2573=VERTEX_POINT('',#8482);
#2574=VERTEX_POINT('',#8484);
#2575=VERTEX_POINT('',#8488);
#2576=VERTEX_POINT('',#8489);
#2577=VERTEX_POINT('',#8494);
#2578=VERTEX_POINT('',#8498);
#2579=VERTEX_POINT('',#8499);
#2580=VERTEX_POINT('',#8504);
#2581=VERTEX_POINT('',#8505);
#2582=VERTEX_POINT('',#8507);
#2583=VERTEX_POINT('',#8509);
#2584=VERTEX_POINT('',#8513);
#2585=VERTEX_POINT('',#8515);
#2586=VERTEX_POINT('',#8522);
#2587=VERTEX_POINT('',#8526);
#2588=VERTEX_POINT('',#8528);
#2589=VERTEX_POINT('',#8530);
#2590=VERTEX_POINT('',#8534);
#2591=VERTEX_POINT('',#8536);
#2592=VERTEX_POINT('',#8540);
#2593=VERTEX_POINT('',#8541);
#2594=VERTEX_POINT('',#8546);
#2595=VERTEX_POINT('',#8547);
#2596=VERTEX_POINT('',#8552);
#2597=VERTEX_POINT('',#8554);
#2598=VERTEX_POINT('',#8558);
#2599=VERTEX_POINT('',#8560);
#2600=VERTEX_POINT('',#8564);
#2601=VERTEX_POINT('',#8566);
#2602=VERTEX_POINT('',#8568);
#2603=VERTEX_POINT('',#8570);
#2604=VERTEX_POINT('',#8572);
#2605=VERTEX_POINT('',#8574);
#2606=VERTEX_POINT('',#8576);
#2607=VERTEX_POINT('',#8578);
#2608=VERTEX_POINT('',#8580);
#2609=VERTEX_POINT('',#8583);
#2610=VERTEX_POINT('',#8586);
#2611=VERTEX_POINT('',#8588);
#2612=VERTEX_POINT('',#8592);
#2613=VERTEX_POINT('',#8593);
#2614=VERTEX_POINT('',#8598);
#2615=VERTEX_POINT('',#8600);
#2616=VERTEX_POINT('',#8602);
#2617=VERTEX_POINT('',#8604);
#2618=VERTEX_POINT('',#8606);
#2619=VERTEX_POINT('',#8608);
#2620=VERTEX_POINT('',#8610);
#2621=VERTEX_POINT('',#8612);
#2622=VERTEX_POINT('',#8614);
#2623=VERTEX_POINT('',#8640);
#2624=VERTEX_POINT('',#8642);
#2625=VERTEX_POINT('',#8646);
#2626=VERTEX_POINT('',#8649);
#2627=VERTEX_POINT('',#8652);
#2628=VERTEX_POINT('',#8656);
#2629=VERTEX_POINT('',#8658);
#2630=VERTEX_POINT('',#8661);
#2631=VERTEX_POINT('',#8670);
#2632=VERTEX_POINT('',#8671);
#2633=VERTEX_POINT('',#8673);
#2634=VERTEX_POINT('',#8675);
#2635=VERTEX_POINT('',#8679);
#2636=VERTEX_POINT('',#8680);
#2637=VERTEX_POINT('',#8682);
#2638=VERTEX_POINT('',#8684);
#2639=VERTEX_POINT('',#8698);
#2640=VERTEX_POINT('',#8700);
#2641=VERTEX_POINT('',#8704);
#2642=VERTEX_POINT('',#8706);
#2643=VERTEX_POINT('',#8710);
#2644=VERTEX_POINT('',#8712);
#2645=VERTEX_POINT('',#8716);
#2646=VERTEX_POINT('',#8718);
#2647=VERTEX_POINT('',#8722);
#2648=VERTEX_POINT('',#8724);
#2649=VERTEX_POINT('',#8728);
#2650=VERTEX_POINT('',#8731);
#2651=VERTEX_POINT('',#8733);
#2652=VERTEX_POINT('',#8737);
#2653=VERTEX_POINT('',#8740);
#2654=VERTEX_POINT('',#8744);
#2655=VERTEX_POINT('',#8748);
#2656=VERTEX_POINT('',#8749);
#2657=VERTEX_POINT('',#8751);
#2658=VERTEX_POINT('',#8753);
#2659=VERTEX_POINT('',#8757);
#2660=VERTEX_POINT('',#8758);
#2661=VERTEX_POINT('',#8760);
#2662=VERTEX_POINT('',#8762);
#2663=VERTEX_POINT('',#8766);
#2664=VERTEX_POINT('',#8767);
#2665=VERTEX_POINT('',#8769);
#2666=VERTEX_POINT('',#8771);
#2667=VERTEX_POINT('',#8775);
#2668=VERTEX_POINT('',#8776);
#2669=VERTEX_POINT('',#8778);
#2670=VERTEX_POINT('',#8780);
#2671=VERTEX_POINT('',#8784);
#2672=VERTEX_POINT('',#8785);
#2673=VERTEX_POINT('',#8787);
#2674=VERTEX_POINT('',#8789);
#2675=VERTEX_POINT('',#8793);
#2676=VERTEX_POINT('',#8794);
#2677=VERTEX_POINT('',#8796);
#2678=VERTEX_POINT('',#8798);
#2679=VERTEX_POINT('',#8802);
#2680=VERTEX_POINT('',#8803);
#2681=VERTEX_POINT('',#8805);
#2682=VERTEX_POINT('',#8807);
#2683=VERTEX_POINT('',#8811);
#2684=VERTEX_POINT('',#8814);
#2685=VERTEX_POINT('',#8826);
#2686=VERTEX_POINT('',#8828);
#2687=VERTEX_POINT('',#8832);
#2688=VERTEX_POINT('',#8834);
#2689=VERTEX_POINT('',#8838);
#2690=VERTEX_POINT('',#8839);
#2691=VERTEX_POINT('',#8841);
#2692=VERTEX_POINT('',#8848);
#2693=VERTEX_POINT('',#8877);
#2694=VERTEX_POINT('',#8879);
#2695=VERTEX_POINT('',#8915);
#2696=VERTEX_POINT('',#8917);
#2697=VERTEX_POINT('',#8924);
#2698=VERTEX_POINT('',#8953);
#2699=VERTEX_POINT('',#8955);
#2700=VERTEX_POINT('',#8984);
#2701=VERTEX_POINT('',#8993);
#2702=VERTEX_POINT('',#8995);
#2703=VERTEX_POINT('',#9002);
#2704=VERTEX_POINT('',#9031);
#2705=VERTEX_POINT('',#9033);
#2706=VERTEX_POINT('',#9062);
#2707=VERTEX_POINT('',#9071);
#2708=VERTEX_POINT('',#9073);
#2709=VERTEX_POINT('',#9080);
#2710=VERTEX_POINT('',#9109);
#2711=VERTEX_POINT('',#9111);
#2712=VERTEX_POINT('',#9140);
#2713=VERTEX_POINT('',#9149);
#2714=VERTEX_POINT('',#9151);
#2715=VERTEX_POINT('',#9156);
#2716=VERTEX_POINT('',#9158);
#2717=VERTEX_POINT('',#9179);
#2718=VERTEX_POINT('',#9188);
#2719=VERTEX_POINT('',#9194);
#2720=VERTEX_POINT('',#9196);
#2721=VERTEX_POINT('',#9229);
#2722=VERTEX_POINT('',#9231);
#2723=VERTEX_POINT('',#9263);
#2724=VERTEX_POINT('',#9268);
#2725=VERTEX_POINT('',#9300);
#2726=VERTEX_POINT('',#9302);
#2727=VERTEX_POINT('',#9334);
#2728=VERTEX_POINT('',#9339);
#2729=VERTEX_POINT('',#9372);
#2730=VERTEX_POINT('',#9401);
#2731=VERTEX_POINT('',#9407);
#2732=VERTEX_POINT('',#9413);
#2733=VERTEX_POINT('',#9422);
#2734=VERTEX_POINT('',#9423);
#2735=VERTEX_POINT('',#9428);
#2736=VERTEX_POINT('',#9454);
#2737=VERTEX_POINT('',#9456);
#2738=VERTEX_POINT('',#9482);
#2739=VERTEX_POINT('',#9489);
#2740=VERTEX_POINT('',#9493);
#2741=VERTEX_POINT('',#9497);
#2742=VERTEX_POINT('',#9504);
#2743=VERTEX_POINT('',#9511);
#2744=VERTEX_POINT('',#9540);
#2745=VERTEX_POINT('',#9606);
#2746=VERTEX_POINT('',#9659);
#2747=VERTEX_POINT('',#9671);
#2748=VERTEX_POINT('',#9733);
#2749=VERTEX_POINT('',#9743);
#2750=VERTEX_POINT('',#9750);
#2751=VERTEX_POINT('',#9779);
#2752=VERTEX_POINT('',#9781);
#2753=VERTEX_POINT('',#9906);
#2754=VERTEX_POINT('',#9913);
#2755=VERTEX_POINT('',#9942);
#2756=VERTEX_POINT('',#9944);
#2757=VERTEX_POINT('',#10069);
#2758=VERTEX_POINT('',#10076);
#2759=VERTEX_POINT('',#10105);
#2760=VERTEX_POINT('',#10107);
#2761=VERTEX_POINT('',#10158);
#2762=VERTEX_POINT('',#10187);
#2763=VERTEX_POINT('',#10194);
#2764=VERTEX_POINT('',#10216);
#2765=VERTEX_POINT('',#10251);
#2766=VERTEX_POINT('',#10279);
#2767=VERTEX_POINT('',#10374);
#2768=VERTEX_POINT('',#10375);
#2769=VERTEX_POINT('',#10377);
#2770=VERTEX_POINT('',#10381);
#2771=VERTEX_POINT('',#10382);
#2772=VERTEX_POINT('',#10384);
#2773=VERTEX_POINT('',#10388);
#2774=VERTEX_POINT('',#10389);
#2775=VERTEX_POINT('',#10391);
#2776=VERTEX_POINT('',#10426);
#2777=VERTEX_POINT('',#10427);
#2778=VERTEX_POINT('',#10429);
#2779=VERTEX_POINT('',#10633);
#2780=VERTEX_POINT('',#10635);
#2781=VERTEX_POINT('',#10639);
#2782=VERTEX_POINT('',#10641);
#2783=VERTEX_POINT('',#10645);
#2784=VERTEX_POINT('',#10647);
#2785=VERTEX_POINT('',#10651);
#2786=VERTEX_POINT('',#10653);
#2787=VERTEX_POINT('',#10657);
#2788=VERTEX_POINT('',#10658);
#2789=VERTEX_POINT('',#10660);
#2790=VERTEX_POINT('',#10662);
#2791=VERTEX_POINT('',#10666);
#2792=VERTEX_POINT('',#10668);
#2793=VERTEX_POINT('',#10672);
#2794=VERTEX_POINT('',#10674);
#2795=VERTEX_POINT('',#10678);
#2796=VERTEX_POINT('',#10680);
#2797=VERTEX_POINT('',#10684);
#2798=VERTEX_POINT('',#10686);
#2799=VERTEX_POINT('',#10693);
#2800=VERTEX_POINT('',#10696);
#2801=VERTEX_POINT('',#10697);
#2802=VERTEX_POINT('',#10699);
#2803=VERTEX_POINT('',#10701);
#2804=VERTEX_POINT('',#10705);
#2805=VERTEX_POINT('',#10707);
#2806=VERTEX_POINT('',#10711);
#2807=VERTEX_POINT('',#10713);
#2808=VERTEX_POINT('',#10717);
#2809=VERTEX_POINT('',#10719);
#2810=VERTEX_POINT('',#10723);
#2811=VERTEX_POINT('',#10725);
#2812=VERTEX_POINT('',#10732);
#2813=VERTEX_POINT('',#10735);
#2814=VERTEX_POINT('',#10739);
#2815=VERTEX_POINT('',#10743);
#2816=VERTEX_POINT('',#10744);
#2817=VERTEX_POINT('',#10746);
#2818=VERTEX_POINT('',#10748);
#2819=VERTEX_POINT('',#10752);
#2820=VERTEX_POINT('',#10753);
#2821=VERTEX_POINT('',#10755);
#2822=VERTEX_POINT('',#10757);
#2823=VERTEX_POINT('',#10761);
#2824=VERTEX_POINT('',#10762);
#2825=VERTEX_POINT('',#10764);
#2826=VERTEX_POINT('',#10766);
#2827=VERTEX_POINT('',#10770);
#2828=VERTEX_POINT('',#10771);
#2829=VERTEX_POINT('',#10773);
#2830=VERTEX_POINT('',#10775);
#2831=VERTEX_POINT('',#10779);
#2832=VERTEX_POINT('',#10780);
#2833=VERTEX_POINT('',#10782);
#2834=VERTEX_POINT('',#10784);
#2835=VERTEX_POINT('',#10788);
#2836=VERTEX_POINT('',#10789);
#2837=VERTEX_POINT('',#10791);
#2838=VERTEX_POINT('',#10793);
#2839=VERTEX_POINT('',#10797);
#2840=VERTEX_POINT('',#10798);
#2841=VERTEX_POINT('',#10800);
#2842=VERTEX_POINT('',#10802);
#2843=VERTEX_POINT('',#10806);
#2844=VERTEX_POINT('',#10809);
#2845=VERTEX_POINT('',#10821);
#2846=VERTEX_POINT('',#10823);
#2847=VERTEX_POINT('',#10827);
#2848=VERTEX_POINT('',#10829);
#2849=VERTEX_POINT('',#10833);
#2850=VERTEX_POINT('',#10834);
#2851=VERTEX_POINT('',#10836);
#2852=VERTEX_POINT('',#10843);
#2853=VERTEX_POINT('',#10872);
#2854=VERTEX_POINT('',#10874);
#2855=VERTEX_POINT('',#10910);
#2856=VERTEX_POINT('',#10912);
#2857=VERTEX_POINT('',#10919);
#2858=VERTEX_POINT('',#10948);
#2859=VERTEX_POINT('',#10950);
#2860=VERTEX_POINT('',#10979);
#2861=VERTEX_POINT('',#10988);
#2862=VERTEX_POINT('',#10990);
#2863=VERTEX_POINT('',#10997);
#2864=VERTEX_POINT('',#11026);
#2865=VERTEX_POINT('',#11028);
#2866=VERTEX_POINT('',#11057);
#2867=VERTEX_POINT('',#11066);
#2868=VERTEX_POINT('',#11068);
#2869=VERTEX_POINT('',#11075);
#2870=VERTEX_POINT('',#11104);
#2871=VERTEX_POINT('',#11106);
#2872=VERTEX_POINT('',#11135);
#2873=VERTEX_POINT('',#11144);
#2874=VERTEX_POINT('',#11146);
#2875=VERTEX_POINT('',#11151);
#2876=VERTEX_POINT('',#11153);
#2877=VERTEX_POINT('',#11174);
#2878=VERTEX_POINT('',#11183);
#2879=VERTEX_POINT('',#11189);
#2880=VERTEX_POINT('',#11191);
#2881=VERTEX_POINT('',#11224);
#2882=VERTEX_POINT('',#11226);
#2883=VERTEX_POINT('',#11258);
#2884=VERTEX_POINT('',#11263);
#2885=VERTEX_POINT('',#11295);
#2886=VERTEX_POINT('',#11297);
#2887=VERTEX_POINT('',#11329);
#2888=VERTEX_POINT('',#11334);
#2889=VERTEX_POINT('',#11367);
#2890=VERTEX_POINT('',#11396);
#2891=VERTEX_POINT('',#11402);
#2892=VERTEX_POINT('',#11408);
#2893=VERTEX_POINT('',#11417);
#2894=VERTEX_POINT('',#11418);
#2895=VERTEX_POINT('',#11423);
#2896=VERTEX_POINT('',#11449);
#2897=VERTEX_POINT('',#11451);
#2898=VERTEX_POINT('',#11477);
#2899=VERTEX_POINT('',#11484);
#2900=VERTEX_POINT('',#11488);
#2901=VERTEX_POINT('',#11492);
#2902=VERTEX_POINT('',#11499);
#2903=VERTEX_POINT('',#11506);
#2904=VERTEX_POINT('',#11535);
#2905=VERTEX_POINT('',#11601);
#2906=VERTEX_POINT('',#11654);
#2907=VERTEX_POINT('',#11666);
#2908=VERTEX_POINT('',#11728);
#2909=VERTEX_POINT('',#11738);
#2910=VERTEX_POINT('',#11745);
#2911=VERTEX_POINT('',#11774);
#2912=VERTEX_POINT('',#11776);
#2913=VERTEX_POINT('',#11901);
#2914=VERTEX_POINT('',#11908);
#2915=VERTEX_POINT('',#11937);
#2916=VERTEX_POINT('',#11939);
#2917=VERTEX_POINT('',#12064);
#2918=VERTEX_POINT('',#12071);
#2919=VERTEX_POINT('',#12100);
#2920=VERTEX_POINT('',#12102);
#2921=VERTEX_POINT('',#12153);
#2922=VERTEX_POINT('',#12182);
#2923=VERTEX_POINT('',#12189);
#2924=VERTEX_POINT('',#12211);
#2925=VERTEX_POINT('',#12246);
#2926=VERTEX_POINT('',#12274);
#2927=VERTEX_POINT('',#12369);
#2928=VERTEX_POINT('',#12370);
#2929=VERTEX_POINT('',#12372);
#2930=VERTEX_POINT('',#12376);
#2931=VERTEX_POINT('',#12377);
#2932=VERTEX_POINT('',#12379);
#2933=VERTEX_POINT('',#12383);
#2934=VERTEX_POINT('',#12384);
#2935=VERTEX_POINT('',#12386);
#2936=VERTEX_POINT('',#12421);
#2937=VERTEX_POINT('',#12422);
#2938=VERTEX_POINT('',#12424);
#2939=VERTEX_POINT('',#12628);
#2940=VERTEX_POINT('',#12630);
#2941=VERTEX_POINT('',#12634);
#2942=VERTEX_POINT('',#12636);
#2943=VERTEX_POINT('',#12640);
#2944=VERTEX_POINT('',#12642);
#2945=VERTEX_POINT('',#12645);
#2946=VERTEX_POINT('',#12650);
#2947=VERTEX_POINT('',#12652);
#2948=VERTEX_POINT('',#12655);
#2949=VERTEX_POINT('',#12660);
#2950=VERTEX_POINT('',#12662);
#2951=VERTEX_POINT('',#12665);
#2952=VERTEX_POINT('',#12670);
#2953=VERTEX_POINT('',#12672);
#2954=VERTEX_POINT('',#12675);
#2955=VERTEX_POINT('',#12680);
#2956=VERTEX_POINT('',#12684);
#2957=VERTEX_POINT('',#12688);
#2958=VERTEX_POINT('',#12692);
#2959=VERTEX_POINT('',#12720);
#2960=VERTEX_POINT('',#12721);
#2961=VERTEX_POINT('',#12723);
#2962=VERTEX_POINT('',#12729);
#2963=VERTEX_POINT('',#12737);
#2964=VERTEX_POINT('',#12738);
#2965=VERTEX_POINT('',#12767);
#2966=VERTEX_POINT('',#12768);
#2967=VERTEX_POINT('',#12810);
#2968=VERTEX_POINT('',#12811);
#2969=VERTEX_POINT('',#12850);
#2970=VERTEX_POINT('',#12851);
#2971=VERTEX_POINT('',#12864);
#2972=VERTEX_POINT('',#12865);
#2973=VERTEX_POINT('',#12894);
#2974=VERTEX_POINT('',#12895);
#2975=VERTEX_POINT('',#12950);
#2976=VERTEX_POINT('',#12955);
#2977=VERTEX_POINT('',#12981);
#2978=VERTEX_POINT('',#13027);
#2979=VERTEX_POINT('',#13056);
#2980=VERTEX_POINT('',#13091);
#2981=VERTEX_POINT('',#13117);
#2982=VERTEX_POINT('',#13167);
#2983=VERTEX_POINT('',#13223);
#2984=VERTEX_POINT('',#13224);
#2985=VERTEX_POINT('',#13226);
#2986=VERTEX_POINT('',#13237);
#2987=VERTEX_POINT('',#13247);
#2988=VERTEX_POINT('',#13248);
#2989=VERTEX_POINT('',#13295);
#2990=VERTEX_POINT('',#13296);
#2991=VERTEX_POINT('',#13343);
#2992=VERTEX_POINT('',#13344);
#2993=VERTEX_POINT('',#13394);
#2994=VERTEX_POINT('',#13395);
#2995=VERTEX_POINT('',#13442);
#2996=VERTEX_POINT('',#13443);
#2997=VERTEX_POINT('',#13490);
#2998=VERTEX_POINT('',#13491);
#2999=VERTEX_POINT('',#13538);
#3000=VERTEX_POINT('',#13539);
#3001=VERTEX_POINT('',#13592);
#3002=VERTEX_POINT('',#13593);
#3003=VERTEX_POINT('',#13640);
#3004=VERTEX_POINT('',#13641);
#3005=VERTEX_POINT('',#13688);
#3006=VERTEX_POINT('',#13689);
#3007=VERTEX_POINT('',#13742);
#3008=VERTEX_POINT('',#13743);
#3009=VERTEX_POINT('',#13790);
#3010=VERTEX_POINT('',#13791);
#3011=VERTEX_POINT('',#13838);
#3012=VERTEX_POINT('',#13839);
#3013=VERTEX_POINT('',#13886);
#3014=VERTEX_POINT('',#13887);
#3015=VERTEX_POINT('',#13940);
#3016=VERTEX_POINT('',#13941);
#3017=VERTEX_POINT('',#13988);
#3018=VERTEX_POINT('',#13989);
#3019=VERTEX_POINT('',#14036);
#3020=VERTEX_POINT('',#14037);
#3021=VERTEX_POINT('',#14090);
#3022=VERTEX_POINT('',#14091);
#3023=VERTEX_POINT('',#14138);
#3024=VERTEX_POINT('',#14139);
#3025=VERTEX_POINT('',#14186);
#3026=VERTEX_POINT('',#14187);
#3027=VERTEX_POINT('',#14240);
#3028=VERTEX_POINT('',#14241);
#3029=VERTEX_POINT('',#14288);
#3030=VERTEX_POINT('',#14289);
#3031=VERTEX_POINT('',#14336);
#3032=VERTEX_POINT('',#14337);
#3033=VERTEX_POINT('',#14384);
#3034=VERTEX_POINT('',#14385);
#3035=VERTEX_POINT('',#14438);
#3036=VERTEX_POINT('',#14439);
#3037=VERTEX_POINT('',#14486);
#3038=VERTEX_POINT('',#14487);
#3039=VERTEX_POINT('',#14534);
#3040=VERTEX_POINT('',#14535);
#3041=VERTEX_POINT('',#14588);
#3042=VERTEX_POINT('',#14589);
#3043=VERTEX_POINT('',#14636);
#3044=VERTEX_POINT('',#14637);
#3045=VERTEX_POINT('',#14684);
#3046=VERTEX_POINT('',#14685);
#3047=VERTEX_POINT('',#14687);
#3048=VERTEX_POINT('',#14698);
#3049=VERTEX_POINT('',#14710);
#3050=VERTEX_POINT('',#14711);
#3051=VERTEX_POINT('',#14734);
#3052=VERTEX_POINT('',#14735);
#3053=VERTEX_POINT('',#14758);
#3054=VERTEX_POINT('',#14759);
#3055=VERTEX_POINT('',#14783);
#3056=VERTEX_POINT('',#14784);
#3057=VERTEX_POINT('',#14808);
#3058=VERTEX_POINT('',#14809);
#3059=VERTEX_POINT('',#14832);
#3060=VERTEX_POINT('',#14833);
#3061=VERTEX_POINT('',#14857);
#3062=VERTEX_POINT('',#14858);
#3063=VERTEX_POINT('',#14882);
#3064=VERTEX_POINT('',#14883);
#3065=VERTEX_POINT('',#14906);
#3066=VERTEX_POINT('',#14907);
#3067=VERTEX_POINT('',#14930);
#3068=VERTEX_POINT('',#14931);
#3069=VERTEX_POINT('',#14955);
#3070=VERTEX_POINT('',#14956);
#3071=VERTEX_POINT('',#14980);
#3072=VERTEX_POINT('',#14981);
#3073=VERTEX_POINT('',#15004);
#3074=VERTEX_POINT('',#15005);
#3075=VERTEX_POINT('',#15029);
#3076=VERTEX_POINT('',#15030);
#3077=VERTEX_POINT('',#15054);
#3078=VERTEX_POINT('',#15055);
#3079=VERTEX_POINT('',#15078);
#3080=VERTEX_POINT('',#15079);
#3081=VERTEX_POINT('',#15103);
#3082=VERTEX_POINT('',#15104);
#3083=VERTEX_POINT('',#15128);
#3084=VERTEX_POINT('',#15129);
#3085=VERTEX_POINT('',#15152);
#3086=VERTEX_POINT('',#15153);
#3087=VERTEX_POINT('',#15176);
#3088=VERTEX_POINT('',#15177);
#3089=VERTEX_POINT('',#15201);
#3090=VERTEX_POINT('',#15202);
#3091=VERTEX_POINT('',#15226);
#3092=VERTEX_POINT('',#15227);
#3093=VERTEX_POINT('',#15250);
#3094=VERTEX_POINT('',#15251);
#3095=VERTEX_POINT('',#15275);
#3096=VERTEX_POINT('',#15276);
#3097=VERTEX_POINT('',#15300);
#3098=VERTEX_POINT('',#15301);
#3099=VERTEX_POINT('',#15324);
#3100=VERTEX_POINT('',#15325);
#3101=VERTEX_POINT('',#15349);
#3102=VERTEX_POINT('',#15350);
#3103=VERTEX_POINT('',#15373);
#3104=VERTEX_POINT('',#15374);
#3105=VERTEX_POINT('',#15398);
#3106=VERTEX_POINT('',#15399);
#3107=VERTEX_POINT('',#15422);
#3108=VERTEX_POINT('',#15544);
#3109=VERTEX_POINT('',#15582);
#3110=VERTEX_POINT('',#15600);
#3111=VERTEX_POINT('',#16387);
#3112=VERTEX_POINT('',#16465);
#3113=VERTEX_POINT('',#17344);
#3114=VERTEX_POINT('',#17345);
#3115=VERTEX_POINT('',#17347);
#3116=VERTEX_POINT('',#17349);
#3117=VERTEX_POINT('',#17353);
#3118=VERTEX_POINT('',#17355);
#3119=VERTEX_POINT('',#17359);
#3120=VERTEX_POINT('',#17361);
#3121=VERTEX_POINT('',#17365);
#3122=VERTEX_POINT('',#17367);
#3123=VERTEX_POINT('',#17371);
#3124=VERTEX_POINT('',#17373);
#3125=VERTEX_POINT('',#17381);
#3126=VERTEX_POINT('',#17384);
#3127=VERTEX_POINT('',#17391);
#3128=VERTEX_POINT('',#17392);
#3129=VERTEX_POINT('',#17394);
#3130=VERTEX_POINT('',#17404);
#3131=VERTEX_POINT('',#17405);
#3132=VERTEX_POINT('',#17407);
#3133=VERTEX_POINT('',#17451);
#3134=VERTEX_POINT('',#17452);
#3135=VERTEX_POINT('',#17505);
#3136=VERTEX_POINT('',#17506);
#3137=VERTEX_POINT('',#17553);
#3138=VERTEX_POINT('',#17554);
#3139=VERTEX_POINT('',#17556);
#3140=VERTEX_POINT('',#17570);
#3141=VERTEX_POINT('',#17592);
#3142=VERTEX_POINT('',#17593);
#3143=VERTEX_POINT('',#17595);
#3144=VERTEX_POINT('',#17603);
#3145=VERTEX_POINT('',#17613);
#3146=VERTEX_POINT('',#17614);
#3147=VERTEX_POINT('',#17638);
#3148=VERTEX_POINT('',#17639);
#3149=VERTEX_POINT('',#17663);
#3150=VERTEX_POINT('',#17664);
#3151=VERTEX_POINT('',#17688);
#3152=VERTEX_POINT('',#17689);
#3153=VERTEX_POINT('',#17691);
#3154=VERTEX_POINT('',#17697);
#3155=VERTEX_POINT('',#18261);
#3156=VERTEX_POINT('',#18262);
#3157=VERTEX_POINT('',#18264);
#3158=VERTEX_POINT('',#18266);
#3159=VERTEX_POINT('',#18268);
#3160=VERTEX_POINT('',#18270);
#3161=VERTEX_POINT('',#18275);
#3162=VERTEX_POINT('',#18276);
#3163=VERTEX_POINT('',#18281);
#3164=VERTEX_POINT('',#18285);
#3165=VERTEX_POINT('',#18289);
#3166=VERTEX_POINT('',#18293);
#3167=VERTEX_POINT('',#18309);
#3168=VERTEX_POINT('',#18311);
#3169=VERTEX_POINT('',#18315);
#3170=VERTEX_POINT('',#18317);
#3171=EDGE_CURVE('',#2566,#2566,#2399,.T.);
#3172=EDGE_CURVE('',#2566,#2567,#1591,.T.);
#3173=EDGE_CURVE('',#2567,#2567,#2400,.T.);
#3174=EDGE_CURVE('',#2568,#2568,#2401,.T.);
#3175=EDGE_CURVE('',#2568,#2569,#1592,.T.);
#3176=EDGE_CURVE('',#2569,#2569,#2402,.T.);
#3177=EDGE_CURVE('',#2570,#2570,#2403,.T.);
#3178=EDGE_CURVE('',#2570,#2571,#1593,.T.);
#3179=EDGE_CURVE('',#2571,#2571,#2404,.T.);
#3180=EDGE_CURVE('',#2572,#2573,#1594,.T.);
#3181=EDGE_CURVE('',#2574,#2572,#1595,.T.);
#3182=EDGE_CURVE('',#2574,#2573,#1596,.T.);
#3183=EDGE_CURVE('',#2575,#2576,#1597,.T.);
#3184=EDGE_CURVE('',#2575,#2574,#2405,.T.);
#3185=EDGE_CURVE('',#2576,#2572,#2406,.T.);
#3186=EDGE_CURVE('',#2577,#2576,#1598,.T.);
#3187=EDGE_CURVE('',#2575,#2577,#1599,.T.);
#3188=EDGE_CURVE('',#2578,#2579,#1600,.T.);
#3189=EDGE_CURVE('',#2573,#2578,#1601,.T.);
#3190=EDGE_CURVE('',#2579,#2574,#1602,.T.);
#3191=EDGE_CURVE('',#2580,#2581,#1603,.T.);
#3192=EDGE_CURVE('',#2580,#2582,#1604,.T.);
#3193=EDGE_CURVE('',#2583,#2582,#1605,.T.);
#3194=EDGE_CURVE('',#2581,#2583,#1606,.T.);
#3195=EDGE_CURVE('',#2584,#2575,#2407,.T.);
#3196=EDGE_CURVE('',#2585,#2577,#2408,.T.);
#3197=EDGE_CURVE('',#2584,#2585,#1607,.T.);
#3198=EDGE_CURVE('',#2580,#2584,#2409,.T.);
#3199=EDGE_CURVE('',#2582,#2585,#2410,.T.);
#3200=EDGE_CURVE('',#2586,#2578,#1608,.T.);
#3201=EDGE_CURVE('',#2583,#2586,#1609,.T.);
#3202=EDGE_CURVE('',#2586,#2587,#1610,.T.);
#3203=EDGE_CURVE('',#2588,#2587,#1611,.T.);
#3204=EDGE_CURVE('',#2589,#2588,#1612,.T.);
#3205=EDGE_CURVE('',#2581,#2589,#1613,.T.);
#3206=EDGE_CURVE('',#2590,#2579,#1614,.T.);
#3207=EDGE_CURVE('',#2590,#2591,#1615,.T.);
#3208=EDGE_CURVE('',#2587,#2591,#1616,.T.);
#3209=EDGE_CURVE('',#2592,#2593,#1617,.T.);
#3210=EDGE_CURVE('',#2591,#2592,#1618,.T.);
#3211=EDGE_CURVE('',#2593,#2590,#1619,.T.);
#3212=EDGE_CURVE('',#2594,#2595,#1620,.T.);
#3213=EDGE_CURVE('',#2589,#2594,#1621,.T.);
#3214=EDGE_CURVE('',#2595,#2588,#1622,.T.);
#3215=EDGE_CURVE('',#2593,#2596,#2411,.T.);
#3216=EDGE_CURVE('',#2596,#2597,#1623,.T.);
#3217=EDGE_CURVE('',#2592,#2597,#2412,.T.);
#3218=EDGE_CURVE('',#2598,#2595,#2413,.T.);
#3219=EDGE_CURVE('',#2598,#2599,#1624,.T.);
#3220=EDGE_CURVE('',#2599,#2594,#2414,.T.);
#3221=EDGE_CURVE('',#2597,#2600,#1625,.T.);
#3222=EDGE_CURVE('',#2600,#2601,#2415,.T.);
#3223=EDGE_CURVE('',#2601,#2602,#1626,.T.);
#3224=EDGE_CURVE('',#2602,#2603,#1627,.T.);
#3225=EDGE_CURVE('',#2603,#2604,#1628,.T.);
#3226=EDGE_CURVE('',#2604,#2605,#1629,.T.);
#3227=EDGE_CURVE('',#2605,#2606,#1630,.T.);
#3228=EDGE_CURVE('',#2606,#2607,#2416,.T.);
#3229=EDGE_CURVE('',#2607,#2608,#1631,.T.);
#3230=EDGE_CURVE('',#2608,#2598,#1632,.T.);
#3231=EDGE_CURVE('',#2609,#2609,#2417,.T.);
#3232=EDGE_CURVE('',#2610,#2610,#2418,.T.);
#3233=EDGE_CURVE('',#2610,#2611,#2419,.T.);
#3234=EDGE_CURVE('',#2611,#2611,#2420,.T.);
#3235=EDGE_CURVE('',#2612,#2613,#2421,.T.);
#3236=EDGE_CURVE('',#2613,#2612,#2422,.T.);
#3237=EDGE_CURVE('',#2613,#2611,#1633,.T.);
#3238=EDGE_CURVE('',#2614,#2599,#1634,.T.);
#3239=EDGE_CURVE('',#2615,#2614,#1635,.T.);
#3240=EDGE_CURVE('',#2616,#2615,#2423,.T.);
#3241=EDGE_CURVE('',#2617,#2616,#1636,.T.);
#3242=EDGE_CURVE('',#2618,#2617,#1637,.T.);
#3243=EDGE_CURVE('',#2619,#2618,#1638,.T.);
#3244=EDGE_CURVE('',#2620,#2619,#1639,.T.);
#3245=EDGE_CURVE('',#2621,#2620,#1640,.T.);
#3246=EDGE_CURVE('',#2622,#2621,#2424,.T.);
#3247=EDGE_CURVE('',#2596,#2622,#1641,.T.);
#3248=EDGE_CURVE('',#2609,#2612,#2425,.T.);
#3249=EDGE_CURVE('',#2607,#2615,#1642,.T.);
#3250=EDGE_CURVE('',#2616,#2606,#1643,.T.);
#3251=EDGE_CURVE('',#2622,#2600,#1644,.T.);
#3252=EDGE_CURVE('',#2601,#2621,#1645,.T.);
#3253=EDGE_CURVE('',#2620,#2602,#1646,.T.);
#3254=EDGE_CURVE('',#2617,#2605,#1647,.T.);
#3255=EDGE_CURVE('',#2614,#2608,#1648,.T.);
#3256=EDGE_CURVE('',#2618,#2604,#1649,.T.);
#3257=EDGE_CURVE('',#2619,#2603,#1650,.T.);
#3258=EDGE_CURVE('',#2623,#2623,#2426,.T.);
#3259=EDGE_CURVE('',#2623,#2624,#1651,.T.);
#3260=EDGE_CURVE('',#2624,#2624,#2427,.T.);
#3261=EDGE_CURVE('',#2625,#2625,#2428,.T.);
#3262=EDGE_CURVE('',#2626,#2626,#2429,.T.);
#3263=EDGE_CURVE('',#2627,#2627,#2430,.T.);
#3264=EDGE_CURVE('',#2627,#2626,#1652,.T.);
#3265=EDGE_CURVE('',#2628,#2628,#2431,.T.);
#3266=EDGE_CURVE('',#2629,#2629,#2432,.T.);
#3267=EDGE_CURVE('',#2628,#2630,#1653,.T.);
#3268=EDGE_CURVE('',#2630,#2630,#2433,.T.);
#3269=EDGE_CURVE('',#2625,#2629,#1654,.T.);
#3270=EDGE_CURVE('',#2631,#2632,#1655,.T.);
#3271=EDGE_CURVE('',#2633,#2631,#1656,.T.);
#3272=EDGE_CURVE('',#2634,#2633,#1657,.T.);
#3273=EDGE_CURVE('',#2632,#2634,#1658,.T.);
#3274=EDGE_CURVE('',#2635,#2636,#1659,.T.);
#3275=EDGE_CURVE('',#2637,#2635,#1660,.T.);
#3276=EDGE_CURVE('',#2638,#2637,#1661,.T.);
#3277=EDGE_CURVE('',#2636,#2638,#1662,.T.);
#3278=EDGE_CURVE('',#2633,#2638,#2434,.T.);
#3279=EDGE_CURVE('',#2636,#2631,#2435,.T.);
#3280=EDGE_CURVE('',#2635,#2632,#2436,.T.);
#3281=EDGE_CURVE('',#2634,#2637,#2437,.T.);
#3282=EDGE_CURVE('',#2639,#2639,#2438,.T.);
#3283=EDGE_CURVE('',#2639,#2640,#1663,.T.);
#3284=EDGE_CURVE('',#2640,#2640,#2439,.T.);
#3285=EDGE_CURVE('',#2641,#2641,#2440,.T.);
#3286=EDGE_CURVE('',#2641,#2642,#1664,.T.);
#3287=EDGE_CURVE('',#2642,#2642,#2441,.T.);
#3288=EDGE_CURVE('',#2643,#2643,#2442,.T.);
#3289=EDGE_CURVE('',#2643,#2644,#1665,.T.);
#3290=EDGE_CURVE('',#2644,#2644,#2443,.T.);
#3291=EDGE_CURVE('',#2645,#2645,#2444,.T.);
#3292=EDGE_CURVE('',#2645,#2646,#1666,.T.);
#3293=EDGE_CURVE('',#2646,#2646,#2445,.T.);
#3294=EDGE_CURVE('',#2647,#2647,#2446,.T.);
#3295=EDGE_CURVE('',#2647,#2648,#1667,.T.);
#3296=EDGE_CURVE('',#2648,#2648,#2447,.T.);
#3297=EDGE_CURVE('',#2649,#2649,#2448,.T.);
#3298=EDGE_CURVE('',#2650,#2650,#2449,.T.);
#3299=EDGE_CURVE('',#2650,#2651,#1668,.T.);
#3300=EDGE_CURVE('',#2651,#2651,#2450,.T.);
#3301=EDGE_CURVE('',#2652,#2652,#2451,.T.);
#3302=EDGE_CURVE('',#2649,#2653,#1669,.T.);
#3303=EDGE_CURVE('',#2653,#2653,#2452,.T.);
#3304=EDGE_CURVE('',#2652,#2654,#1670,.T.);
#3305=EDGE_CURVE('',#2654,#2654,#2453,.T.);
#3306=EDGE_CURVE('',#2655,#2656,#1671,.T.);
#3307=EDGE_CURVE('',#2657,#2655,#1672,.T.);
#3308=EDGE_CURVE('',#2658,#2657,#1673,.T.);
#3309=EDGE_CURVE('',#2658,#2656,#1674,.T.);
#3310=EDGE_CURVE('',#2659,#2660,#1675,.T.);
#3311=EDGE_CURVE('',#2659,#2661,#1676,.T.);
#3312=EDGE_CURVE('',#2662,#2661,#1677,.T.);
#3313=EDGE_CURVE('',#2660,#2662,#1678,.T.);
#3314=EDGE_CURVE('',#2663,#2664,#1679,.T.);
#3315=EDGE_CURVE('',#2663,#2665,#1680,.T.);
#3316=EDGE_CURVE('',#2666,#2665,#1681,.T.);
#3317=EDGE_CURVE('',#2664,#2666,#1682,.T.);
#3318=EDGE_CURVE('',#2667,#2668,#1683,.T.);
#3319=EDGE_CURVE('',#2667,#2669,#1684,.T.);
#3320=EDGE_CURVE('',#2670,#2669,#1685,.T.);
#3321=EDGE_CURVE('',#2668,#2670,#1686,.T.);
#3322=EDGE_CURVE('',#2671,#2672,#1687,.T.);
#3323=EDGE_CURVE('',#2671,#2673,#1688,.T.);
#3324=EDGE_CURVE('',#2674,#2673,#1689,.T.);
#3325=EDGE_CURVE('',#2672,#2674,#1690,.T.);
#3326=EDGE_CURVE('',#2675,#2676,#1691,.T.);
#3327=EDGE_CURVE('',#2677,#2675,#1692,.T.);
#3328=EDGE_CURVE('',#2678,#2677,#1693,.T.);
#3329=EDGE_CURVE('',#2678,#2676,#1694,.T.);
#3330=EDGE_CURVE('',#2679,#2680,#1695,.T.);
#3331=EDGE_CURVE('',#2681,#2679,#1696,.T.);
#3332=EDGE_CURVE('',#2682,#2681,#1697,.T.);
#3333=EDGE_CURVE('',#2682,#2680,#1698,.T.);
#3334=EDGE_CURVE('',#2683,#2683,#2454,.T.);
#3335=EDGE_CURVE('',#2684,#2684,#2455,.T.);
#3336=EDGE_CURVE('',#2656,#2671,#1699,.T.);
#3337=EDGE_CURVE('',#2673,#2658,#1700,.T.);
#3338=EDGE_CURVE('',#2676,#2659,#1701,.T.);
#3339=EDGE_CURVE('',#2661,#2678,#1702,.T.);
#3340=EDGE_CURVE('',#2680,#2663,#1703,.T.);
#3341=EDGE_CURVE('',#2665,#2682,#1704,.T.);
#3342=EDGE_CURVE('',#2685,#2667,#1705,.T.);
#3343=EDGE_CURVE('',#2686,#2685,#1706,.T.);
#3344=EDGE_CURVE('',#2669,#2686,#1707,.T.);
#3345=EDGE_CURVE('',#2687,#2685,#1708,.T.);
#3346=EDGE_CURVE('',#2688,#2687,#1709,.T.);
#3347=EDGE_CURVE('',#2686,#2688,#1710,.T.);
#3348=EDGE_CURVE('',#2689,#2690,#1711,.T.);
#3349=EDGE_CURVE('',#2691,#2690,#171,.T.);
#3350=EDGE_CURVE('',#2692,#2691,#172,.T.);
#3351=EDGE_CURVE('',#2693,#2692,#1712,.T.);
#3352=EDGE_CURVE('',#2694,#2693,#173,.T.);
#3353=EDGE_CURVE('',#2689,#2694,#174,.T.);
#3354=EDGE_CURVE('',#2688,#2695,#1713,.T.);
#3355=EDGE_CURVE('',#2696,#2695,#175,.T.);
#3356=EDGE_CURVE('',#2697,#2696,#176,.T.);
#3357=EDGE_CURVE('',#2698,#2697,#1714,.T.);
#3358=EDGE_CURVE('',#2699,#2698,#177,.T.);
#3359=EDGE_CURVE('',#2700,#2699,#178,.T.);
#3360=EDGE_CURVE('',#2700,#2670,#1715,.T.);
#3361=EDGE_CURVE('',#2681,#2701,#1716,.T.);
#3362=EDGE_CURVE('',#2702,#2701,#179,.T.);
#3363=EDGE_CURVE('',#2703,#2702,#180,.T.);
#3364=EDGE_CURVE('',#2704,#2703,#1717,.T.);
#3365=EDGE_CURVE('',#2705,#2704,#181,.T.);
#3366=EDGE_CURVE('',#2706,#2705,#182,.T.);
#3367=EDGE_CURVE('',#2706,#2666,#1718,.T.);
#3368=EDGE_CURVE('',#2677,#2707,#1719,.T.);
#3369=EDGE_CURVE('',#2708,#2707,#183,.T.);
#3370=EDGE_CURVE('',#2709,#2708,#184,.T.);
#3371=EDGE_CURVE('',#2710,#2709,#1720,.T.);
#3372=EDGE_CURVE('',#2711,#2710,#185,.T.);
#3373=EDGE_CURVE('',#2712,#2711,#186,.T.);
#3374=EDGE_CURVE('',#2712,#2662,#1721,.T.);
#3375=EDGE_CURVE('',#2713,#2672,#1722,.T.);
#3376=EDGE_CURVE('',#2713,#2714,#187,.T.);
#3377=EDGE_CURVE('',#2714,#2715,#1723,.T.);
#3378=EDGE_CURVE('',#2715,#2716,#188,.T.);
#3379=EDGE_CURVE('',#2655,#2716,#1724,.T.);
#3380=EDGE_CURVE('',#2700,#2690,#189,.T.);
#3381=EDGE_CURVE('',#2689,#2695,#190,.T.);
#3382=EDGE_CURVE('',#2717,#2687,#1725,.T.);
#3383=EDGE_CURVE('',#2717,#2701,#191,.T.);
#3384=EDGE_CURVE('',#2718,#2679,#1726,.T.);
#3385=EDGE_CURVE('',#2718,#2707,#192,.T.);
#3386=EDGE_CURVE('',#2719,#2675,#1727,.T.);
#3387=EDGE_CURVE('',#2719,#2720,#193,.T.);
#3388=EDGE_CURVE('',#2720,#2713,#194,.T.);
#3389=EDGE_CURVE('',#2674,#2721,#1728,.T.);
#3390=EDGE_CURVE('',#2722,#2721,#195,.T.);
#3391=EDGE_CURVE('',#2722,#2723,#196,.T.);
#3392=EDGE_CURVE('',#2724,#2723,#197,.T.);
#3393=EDGE_CURVE('',#2724,#2725,#1729,.T.);
#3394=EDGE_CURVE('',#2726,#2725,#198,.T.);
#3395=EDGE_CURVE('',#2726,#2727,#199,.T.);
#3396=EDGE_CURVE('',#2728,#2727,#200,.T.);
#3397=EDGE_CURVE('',#2728,#2657,#1730,.T.);
#3398=EDGE_CURVE('',#2716,#2729,#201,.T.);
#3399=EDGE_CURVE('',#2729,#2730,#202,.T.);
#3400=EDGE_CURVE('',#2660,#2730,#1731,.T.);
#3401=EDGE_CURVE('',#2712,#2731,#203,.T.);
#3402=EDGE_CURVE('',#2664,#2731,#1732,.T.);
#3403=EDGE_CURVE('',#2706,#2732,#204,.T.);
#3404=EDGE_CURVE('',#2668,#2732,#1733,.T.);
#3405=EDGE_CURVE('',#2733,#2734,#205,.T.);
#3406=EDGE_CURVE('',#2734,#2735,#206,.T.);
#3407=EDGE_CURVE('',#2735,#2736,#1734,.T.);
#3408=EDGE_CURVE('',#2736,#2737,#207,.T.);
#3409=EDGE_CURVE('',#2737,#2738,#208,.T.);
#3410=EDGE_CURVE('',#2733,#2738,#1735,.T.);
#3411=EDGE_CURVE('',#2739,#2739,#2456,.T.);
#3412=EDGE_CURVE('',#2739,#2684,#1736,.T.);
#3413=EDGE_CURVE('',#2740,#2740,#2457,.T.);
#3414=EDGE_CURVE('',#2740,#2683,#1737,.T.);
#3415=EDGE_CURVE('',#2733,#2741,#209,.T.);
#3416=EDGE_CURVE('',#2742,#2738,#210,.T.);
#3417=EDGE_CURVE('',#2743,#2742,#211,.T.);
#3418=EDGE_CURVE('',#2744,#2743,#1738,.T.);
#3419=EDGE_CURVE('',#2741,#2744,#212,.T.);
#3420=EDGE_CURVE('',#2699,#2691,#213,.T.);
#3421=EDGE_CURVE('',#2741,#2745,#214,.T.);
#3422=EDGE_CURVE('',#2745,#2734,#215,.T.);
#3423=EDGE_CURVE('',#2692,#2698,#216,.T.);
#3424=EDGE_CURVE('',#2746,#2744,#217,.T.);
#3425=EDGE_CURVE('',#2745,#2746,#2458,.F.);
#3426=EDGE_CURVE('',#2697,#2693,#218,.T.);
#3427=EDGE_CURVE('',#2743,#2747,#219,.T.);
#3428=EDGE_CURVE('',#2747,#2746,#1739,.T.);
#3429=EDGE_CURVE('',#2694,#2696,#220,.T.);
#3430=EDGE_CURVE('',#2737,#2748,#221,.T.);
#3431=EDGE_CURVE('',#2748,#2742,#222,.T.);
#3432=EDGE_CURVE('',#2749,#2732,#223,.T.);
#3433=EDGE_CURVE('',#2750,#2749,#224,.T.);
#3434=EDGE_CURVE('',#2751,#2750,#1740,.T.);
#3435=EDGE_CURVE('',#2752,#2751,#225,.T.);
#3436=EDGE_CURVE('',#2717,#2752,#226,.T.);
#3437=EDGE_CURVE('',#2705,#2749,#227,.T.);
#3438=EDGE_CURVE('',#2750,#2704,#228,.T.);
#3439=EDGE_CURVE('',#2703,#2751,#229,.T.);
#3440=EDGE_CURVE('',#2752,#2702,#230,.T.);
#3441=EDGE_CURVE('',#2753,#2731,#231,.T.);
#3442=EDGE_CURVE('',#2754,#2753,#232,.T.);
#3443=EDGE_CURVE('',#2755,#2754,#1741,.T.);
#3444=EDGE_CURVE('',#2756,#2755,#233,.T.);
#3445=EDGE_CURVE('',#2718,#2756,#234,.T.);
#3446=EDGE_CURVE('',#2711,#2753,#235,.T.);
#3447=EDGE_CURVE('',#2754,#2710,#236,.T.);
#3448=EDGE_CURVE('',#2709,#2755,#237,.T.);
#3449=EDGE_CURVE('',#2756,#2708,#238,.T.);
#3450=EDGE_CURVE('',#2757,#2730,#239,.T.);
#3451=EDGE_CURVE('',#2758,#2757,#240,.T.);
#3452=EDGE_CURVE('',#2759,#2758,#1742,.T.);
#3453=EDGE_CURVE('',#2760,#2759,#241,.T.);
#3454=EDGE_CURVE('',#2719,#2760,#242,.T.);
#3455=EDGE_CURVE('',#2729,#2761,#243,.T.);
#3456=EDGE_CURVE('',#2761,#2757,#244,.T.);
#3457=EDGE_CURVE('',#2762,#2761,#2459,.F.);
#3458=EDGE_CURVE('',#2758,#2762,#245,.T.);
#3459=EDGE_CURVE('',#2762,#2763,#1743,.T.);
#3460=EDGE_CURVE('',#2763,#2759,#246,.T.);
#3461=EDGE_CURVE('',#2760,#2764,#247,.T.);
#3462=EDGE_CURVE('',#2764,#2720,#248,.T.);
#3463=EDGE_CURVE('',#2764,#2763,#2460,.F.);
#3464=EDGE_CURVE('',#2763,#2714,#2461,.F.);
#3465=EDGE_CURVE('',#2714,#2764,#2462,.F.);
#3466=EDGE_CURVE('',#2747,#2748,#2463,.F.);
#3467=EDGE_CURVE('',#2748,#2765,#2464,.F.);
#3468=EDGE_CURVE('',#2765,#2747,#2465,.F.);
#3469=EDGE_CURVE('',#2761,#2715,#2466,.F.);
#3470=EDGE_CURVE('',#2715,#2762,#2467,.F.);
#3471=EDGE_CURVE('',#2766,#2745,#2468,.F.);
#3472=EDGE_CURVE('',#2746,#2766,#2469,.F.);
#3473=EDGE_CURVE('',#2766,#2765,#1744,.T.);
#3474=EDGE_CURVE('',#2735,#2766,#249,.T.);
#3475=EDGE_CURVE('',#2765,#2736,#250,.T.);
#3476=EDGE_CURVE('',#2767,#2768,#2470,.F.);
#3477=EDGE_CURVE('',#2769,#2767,#2471,.F.);
#3478=EDGE_CURVE('',#2768,#2769,#2472,.F.);
#3479=EDGE_CURVE('',#2770,#2771,#2473,.F.);
#3480=EDGE_CURVE('',#2772,#2770,#2474,.F.);
#3481=EDGE_CURVE('',#2771,#2772,#2475,.F.);
#3482=EDGE_CURVE('',#2773,#2774,#2476,.F.);
#3483=EDGE_CURVE('',#2775,#2773,#2477,.F.);
#3484=EDGE_CURVE('',#2774,#2775,#2478,.F.);
#3485=EDGE_CURVE('',#2768,#2775,#1745,.T.);
#3486=EDGE_CURVE('',#2773,#2767,#1746,.T.);
#3487=EDGE_CURVE('',#2727,#2774,#251,.T.);
#3488=EDGE_CURVE('',#2775,#2728,#252,.T.);
#3489=EDGE_CURVE('',#2776,#2777,#2479,.F.);
#3490=EDGE_CURVE('',#2778,#2776,#2480,.F.);
#3491=EDGE_CURVE('',#2777,#2778,#2481,.F.);
#3492=EDGE_CURVE('',#2776,#2772,#1747,.T.);
#3493=EDGE_CURVE('',#2770,#2778,#1748,.T.);
#3494=EDGE_CURVE('',#2774,#2777,#253,.T.);
#3495=EDGE_CURVE('',#2778,#2773,#254,.T.);
#3496=EDGE_CURVE('',#2725,#2776,#255,.T.);
#3497=EDGE_CURVE('',#2777,#2726,#256,.T.);
#3498=EDGE_CURVE('',#2723,#2771,#257,.T.);
#3499=EDGE_CURVE('',#2772,#2724,#258,.T.);
#3500=EDGE_CURVE('',#2771,#2769,#259,.T.);
#3501=EDGE_CURVE('',#2767,#2770,#260,.T.);
#3502=EDGE_CURVE('',#2721,#2768,#261,.T.);
#3503=EDGE_CURVE('',#2769,#2722,#262,.T.);
#3504=EDGE_CURVE('',#2779,#2779,#2482,.T.);
#3505=EDGE_CURVE('',#2779,#2780,#1749,.T.);
#3506=EDGE_CURVE('',#2780,#2780,#2483,.T.);
#3507=EDGE_CURVE('',#2781,#2781,#2484,.T.);
#3508=EDGE_CURVE('',#2781,#2782,#1750,.T.);
#3509=EDGE_CURVE('',#2782,#2782,#2485,.T.);
#3510=EDGE_CURVE('',#2783,#2783,#2486,.T.);
#3511=EDGE_CURVE('',#2783,#2784,#1751,.T.);
#3512=EDGE_CURVE('',#2784,#2784,#2487,.T.);
#3513=EDGE_CURVE('',#2785,#2785,#2488,.T.);
#3514=EDGE_CURVE('',#2785,#2786,#1752,.T.);
#3515=EDGE_CURVE('',#2786,#2786,#2489,.T.);
#3516=EDGE_CURVE('',#2787,#2788,#1753,.T.);
#3517=EDGE_CURVE('',#2787,#2789,#1754,.T.);
#3518=EDGE_CURVE('',#2789,#2790,#1755,.T.);
#3519=EDGE_CURVE('',#2788,#2790,#1756,.T.);
#3520=EDGE_CURVE('',#2791,#2787,#1757,.T.);
#3521=EDGE_CURVE('',#2791,#2792,#1758,.T.);
#3522=EDGE_CURVE('',#2792,#2789,#1759,.T.);
#3523=EDGE_CURVE('',#2793,#2791,#1760,.T.);
#3524=EDGE_CURVE('',#2793,#2794,#1761,.T.);
#3525=EDGE_CURVE('',#2794,#2792,#1762,.T.);
#3526=EDGE_CURVE('',#2795,#2793,#1763,.T.);
#3527=EDGE_CURVE('',#2795,#2796,#1764,.T.);
#3528=EDGE_CURVE('',#2796,#2794,#1765,.T.);
#3529=EDGE_CURVE('',#2797,#2795,#1766,.T.);
#3530=EDGE_CURVE('',#2797,#2798,#1767,.T.);
#3531=EDGE_CURVE('',#2798,#2796,#1768,.T.);
#3532=EDGE_CURVE('',#2788,#2797,#1769,.T.);
#3533=EDGE_CURVE('',#2790,#2798,#1770,.T.);
#3534=EDGE_CURVE('',#2799,#2799,#2490,.T.);
#3535=EDGE_CURVE('',#2800,#2801,#1771,.T.);
#3536=EDGE_CURVE('',#2800,#2802,#1772,.T.);
#3537=EDGE_CURVE('',#2802,#2803,#1773,.T.);
#3538=EDGE_CURVE('',#2801,#2803,#1774,.T.);
#3539=EDGE_CURVE('',#2804,#2800,#1775,.T.);
#3540=EDGE_CURVE('',#2804,#2805,#1776,.T.);
#3541=EDGE_CURVE('',#2805,#2802,#1777,.T.);
#3542=EDGE_CURVE('',#2806,#2804,#1778,.T.);
#3543=EDGE_CURVE('',#2806,#2807,#1779,.T.);
#3544=EDGE_CURVE('',#2807,#2805,#1780,.T.);
#3545=EDGE_CURVE('',#2808,#2806,#1781,.T.);
#3546=EDGE_CURVE('',#2808,#2809,#1782,.T.);
#3547=EDGE_CURVE('',#2809,#2807,#1783,.T.);
#3548=EDGE_CURVE('',#2810,#2808,#1784,.T.);
#3549=EDGE_CURVE('',#2810,#2811,#1785,.T.);
#3550=EDGE_CURVE('',#2811,#2809,#1786,.T.);
#3551=EDGE_CURVE('',#2801,#2810,#1787,.T.);
#3552=EDGE_CURVE('',#2803,#2811,#1788,.T.);
#3553=EDGE_CURVE('',#2812,#2812,#2491,.T.);
#3554=EDGE_CURVE('',#2812,#2813,#1789,.T.);
#3555=EDGE_CURVE('',#2813,#2813,#2492,.T.);
#3556=EDGE_CURVE('',#2799,#2814,#1790,.T.);
#3557=EDGE_CURVE('',#2814,#2814,#2493,.T.);
#3558=EDGE_CURVE('',#2815,#2816,#1791,.T.);
#3559=EDGE_CURVE('',#2817,#2815,#1792,.T.);
#3560=EDGE_CURVE('',#2818,#2817,#1793,.T.);
#3561=EDGE_CURVE('',#2818,#2816,#1794,.T.);
#3562=EDGE_CURVE('',#2819,#2820,#1795,.T.);
#3563=EDGE_CURVE('',#2819,#2821,#1796,.T.);
#3564=EDGE_CURVE('',#2822,#2821,#1797,.T.);
#3565=EDGE_CURVE('',#2820,#2822,#1798,.T.);
#3566=EDGE_CURVE('',#2823,#2824,#1799,.T.);
#3567=EDGE_CURVE('',#2823,#2825,#1800,.T.);
#3568=EDGE_CURVE('',#2826,#2825,#1801,.T.);
#3569=EDGE_CURVE('',#2824,#2826,#1802,.T.);
#3570=EDGE_CURVE('',#2827,#2828,#1803,.T.);
#3571=EDGE_CURVE('',#2827,#2829,#1804,.T.);
#3572=EDGE_CURVE('',#2830,#2829,#1805,.T.);
#3573=EDGE_CURVE('',#2828,#2830,#1806,.T.);
#3574=EDGE_CURVE('',#2831,#2832,#1807,.T.);
#3575=EDGE_CURVE('',#2831,#2833,#1808,.T.);
#3576=EDGE_CURVE('',#2834,#2833,#1809,.T.);
#3577=EDGE_CURVE('',#2832,#2834,#1810,.T.);
#3578=EDGE_CURVE('',#2835,#2836,#1811,.T.);
#3579=EDGE_CURVE('',#2837,#2835,#1812,.T.);
#3580=EDGE_CURVE('',#2838,#2837,#1813,.T.);
#3581=EDGE_CURVE('',#2838,#2836,#1814,.T.);
#3582=EDGE_CURVE('',#2839,#2840,#1815,.T.);
#3583=EDGE_CURVE('',#2841,#2839,#1816,.T.);
#3584=EDGE_CURVE('',#2842,#2841,#1817,.T.);
#3585=EDGE_CURVE('',#2842,#2840,#1818,.T.);
#3586=EDGE_CURVE('',#2843,#2843,#2494,.T.);
#3587=EDGE_CURVE('',#2844,#2844,#2495,.T.);
#3588=EDGE_CURVE('',#2816,#2831,#1819,.T.);
#3589=EDGE_CURVE('',#2833,#2818,#1820,.T.);
#3590=EDGE_CURVE('',#2836,#2819,#1821,.T.);
#3591=EDGE_CURVE('',#2821,#2838,#1822,.T.);
#3592=EDGE_CURVE('',#2840,#2823,#1823,.T.);
#3593=EDGE_CURVE('',#2825,#2842,#1824,.T.);
#3594=EDGE_CURVE('',#2845,#2827,#1825,.T.);
#3595=EDGE_CURVE('',#2846,#2845,#1826,.T.);
#3596=EDGE_CURVE('',#2829,#2846,#1827,.T.);
#3597=EDGE_CURVE('',#2847,#2845,#1828,.T.);
#3598=EDGE_CURVE('',#2848,#2847,#1829,.T.);
#3599=EDGE_CURVE('',#2846,#2848,#1830,.T.);
#3600=EDGE_CURVE('',#2849,#2850,#1831,.T.);
#3601=EDGE_CURVE('',#2851,#2850,#263,.T.);
#3602=EDGE_CURVE('',#2852,#2851,#264,.T.);
#3603=EDGE_CURVE('',#2853,#2852,#1832,.T.);
#3604=EDGE_CURVE('',#2854,#2853,#265,.T.);
#3605=EDGE_CURVE('',#2849,#2854,#266,.T.);
#3606=EDGE_CURVE('',#2848,#2855,#1833,.T.);
#3607=EDGE_CURVE('',#2856,#2855,#267,.T.);
#3608=EDGE_CURVE('',#2857,#2856,#268,.T.);
#3609=EDGE_CURVE('',#2858,#2857,#1834,.T.);
#3610=EDGE_CURVE('',#2859,#2858,#269,.T.);
#3611=EDGE_CURVE('',#2860,#2859,#270,.T.);
#3612=EDGE_CURVE('',#2860,#2830,#1835,.T.);
#3613=EDGE_CURVE('',#2841,#2861,#1836,.T.);
#3614=EDGE_CURVE('',#2862,#2861,#271,.T.);
#3615=EDGE_CURVE('',#2863,#2862,#272,.T.);
#3616=EDGE_CURVE('',#2864,#2863,#1837,.T.);
#3617=EDGE_CURVE('',#2865,#2864,#273,.T.);
#3618=EDGE_CURVE('',#2866,#2865,#274,.T.);
#3619=EDGE_CURVE('',#2866,#2826,#1838,.T.);
#3620=EDGE_CURVE('',#2837,#2867,#1839,.T.);
#3621=EDGE_CURVE('',#2868,#2867,#275,.T.);
#3622=EDGE_CURVE('',#2869,#2868,#276,.T.);
#3623=EDGE_CURVE('',#2870,#2869,#1840,.T.);
#3624=EDGE_CURVE('',#2871,#2870,#277,.T.);
#3625=EDGE_CURVE('',#2872,#2871,#278,.T.);
#3626=EDGE_CURVE('',#2872,#2822,#1841,.T.);
#3627=EDGE_CURVE('',#2873,#2832,#1842,.T.);
#3628=EDGE_CURVE('',#2873,#2874,#279,.T.);
#3629=EDGE_CURVE('',#2874,#2875,#1843,.T.);
#3630=EDGE_CURVE('',#2875,#2876,#280,.T.);
#3631=EDGE_CURVE('',#2815,#2876,#1844,.T.);
#3632=EDGE_CURVE('',#2860,#2850,#281,.T.);
#3633=EDGE_CURVE('',#2849,#2855,#282,.T.);
#3634=EDGE_CURVE('',#2877,#2847,#1845,.T.);
#3635=EDGE_CURVE('',#2877,#2861,#283,.T.);
#3636=EDGE_CURVE('',#2878,#2839,#1846,.T.);
#3637=EDGE_CURVE('',#2878,#2867,#284,.T.);
#3638=EDGE_CURVE('',#2879,#2835,#1847,.T.);
#3639=EDGE_CURVE('',#2879,#2880,#285,.T.);
#3640=EDGE_CURVE('',#2880,#2873,#286,.T.);
#3641=EDGE_CURVE('',#2834,#2881,#1848,.T.);
#3642=EDGE_CURVE('',#2882,#2881,#287,.T.);
#3643=EDGE_CURVE('',#2882,#2883,#288,.T.);
#3644=EDGE_CURVE('',#2884,#2883,#289,.T.);
#3645=EDGE_CURVE('',#2884,#2885,#1849,.T.);
#3646=EDGE_CURVE('',#2886,#2885,#290,.T.);
#3647=EDGE_CURVE('',#2886,#2887,#291,.T.);
#3648=EDGE_CURVE('',#2888,#2887,#292,.T.);
#3649=EDGE_CURVE('',#2888,#2817,#1850,.T.);
#3650=EDGE_CURVE('',#2876,#2889,#293,.T.);
#3651=EDGE_CURVE('',#2889,#2890,#294,.T.);
#3652=EDGE_CURVE('',#2820,#2890,#1851,.T.);
#3653=EDGE_CURVE('',#2872,#2891,#295,.T.);
#3654=EDGE_CURVE('',#2824,#2891,#1852,.T.);
#3655=EDGE_CURVE('',#2866,#2892,#296,.T.);
#3656=EDGE_CURVE('',#2828,#2892,#1853,.T.);
#3657=EDGE_CURVE('',#2893,#2894,#297,.T.);
#3658=EDGE_CURVE('',#2894,#2895,#298,.T.);
#3659=EDGE_CURVE('',#2895,#2896,#1854,.T.);
#3660=EDGE_CURVE('',#2896,#2897,#299,.T.);
#3661=EDGE_CURVE('',#2897,#2898,#300,.T.);
#3662=EDGE_CURVE('',#2893,#2898,#1855,.T.);
#3663=EDGE_CURVE('',#2899,#2899,#2496,.T.);
#3664=EDGE_CURVE('',#2899,#2844,#1856,.T.);
#3665=EDGE_CURVE('',#2900,#2900,#2497,.T.);
#3666=EDGE_CURVE('',#2900,#2843,#1857,.T.);
#3667=EDGE_CURVE('',#2893,#2901,#301,.T.);
#3668=EDGE_CURVE('',#2902,#2898,#302,.T.);
#3669=EDGE_CURVE('',#2903,#2902,#303,.T.);
#3670=EDGE_CURVE('',#2904,#2903,#1858,.T.);
#3671=EDGE_CURVE('',#2901,#2904,#304,.T.);
#3672=EDGE_CURVE('',#2859,#2851,#305,.T.);
#3673=EDGE_CURVE('',#2901,#2905,#306,.T.);
#3674=EDGE_CURVE('',#2905,#2894,#307,.T.);
#3675=EDGE_CURVE('',#2852,#2858,#308,.T.);
#3676=EDGE_CURVE('',#2906,#2904,#309,.T.);
#3677=EDGE_CURVE('',#2905,#2906,#2498,.F.);
#3678=EDGE_CURVE('',#2857,#2853,#310,.T.);
#3679=EDGE_CURVE('',#2903,#2907,#311,.T.);
#3680=EDGE_CURVE('',#2907,#2906,#1859,.T.);
#3681=EDGE_CURVE('',#2854,#2856,#312,.T.);
#3682=EDGE_CURVE('',#2897,#2908,#313,.T.);
#3683=EDGE_CURVE('',#2908,#2902,#314,.T.);
#3684=EDGE_CURVE('',#2909,#2892,#315,.T.);
#3685=EDGE_CURVE('',#2910,#2909,#316,.T.);
#3686=EDGE_CURVE('',#2911,#2910,#1860,.T.);
#3687=EDGE_CURVE('',#2912,#2911,#317,.T.);
#3688=EDGE_CURVE('',#2877,#2912,#318,.T.);
#3689=EDGE_CURVE('',#2865,#2909,#319,.T.);
#3690=EDGE_CURVE('',#2910,#2864,#320,.T.);
#3691=EDGE_CURVE('',#2863,#2911,#321,.T.);
#3692=EDGE_CURVE('',#2912,#2862,#322,.T.);
#3693=EDGE_CURVE('',#2913,#2891,#323,.T.);
#3694=EDGE_CURVE('',#2914,#2913,#324,.T.);
#3695=EDGE_CURVE('',#2915,#2914,#1861,.T.);
#3696=EDGE_CURVE('',#2916,#2915,#325,.T.);
#3697=EDGE_CURVE('',#2878,#2916,#326,.T.);
#3698=EDGE_CURVE('',#2871,#2913,#327,.T.);
#3699=EDGE_CURVE('',#2914,#2870,#328,.T.);
#3700=EDGE_CURVE('',#2869,#2915,#329,.T.);
#3701=EDGE_CURVE('',#2916,#2868,#330,.T.);
#3702=EDGE_CURVE('',#2917,#2890,#331,.T.);
#3703=EDGE_CURVE('',#2918,#2917,#332,.T.);
#3704=EDGE_CURVE('',#2919,#2918,#1862,.T.);
#3705=EDGE_CURVE('',#2920,#2919,#333,.T.);
#3706=EDGE_CURVE('',#2879,#2920,#334,.T.);
#3707=EDGE_CURVE('',#2889,#2921,#335,.T.);
#3708=EDGE_CURVE('',#2921,#2917,#336,.T.);
#3709=EDGE_CURVE('',#2922,#2921,#2499,.F.);
#3710=EDGE_CURVE('',#2918,#2922,#337,.T.);
#3711=EDGE_CURVE('',#2922,#2923,#1863,.T.);
#3712=EDGE_CURVE('',#2923,#2919,#338,.T.);
#3713=EDGE_CURVE('',#2920,#2924,#339,.T.);
#3714=EDGE_CURVE('',#2924,#2880,#340,.T.);
#3715=EDGE_CURVE('',#2924,#2923,#2500,.F.);
#3716=EDGE_CURVE('',#2923,#2874,#2501,.F.);
#3717=EDGE_CURVE('',#2874,#2924,#2502,.F.);
#3718=EDGE_CURVE('',#2907,#2908,#2503,.F.);
#3719=EDGE_CURVE('',#2908,#2925,#2504,.F.);
#3720=EDGE_CURVE('',#2925,#2907,#2505,.F.);
#3721=EDGE_CURVE('',#2921,#2875,#2506,.F.);
#3722=EDGE_CURVE('',#2875,#2922,#2507,.F.);
#3723=EDGE_CURVE('',#2926,#2905,#2508,.F.);
#3724=EDGE_CURVE('',#2906,#2926,#2509,.F.);
#3725=EDGE_CURVE('',#2926,#2925,#1864,.T.);
#3726=EDGE_CURVE('',#2895,#2926,#341,.T.);
#3727=EDGE_CURVE('',#2925,#2896,#342,.T.);
#3728=EDGE_CURVE('',#2927,#2928,#2510,.F.);
#3729=EDGE_CURVE('',#2929,#2927,#2511,.F.);
#3730=EDGE_CURVE('',#2928,#2929,#2512,.F.);
#3731=EDGE_CURVE('',#2930,#2931,#2513,.F.);
#3732=EDGE_CURVE('',#2932,#2930,#2514,.F.);
#3733=EDGE_CURVE('',#2931,#2932,#2515,.F.);
#3734=EDGE_CURVE('',#2933,#2934,#2516,.F.);
#3735=EDGE_CURVE('',#2935,#2933,#2517,.F.);
#3736=EDGE_CURVE('',#2934,#2935,#2518,.F.);
#3737=EDGE_CURVE('',#2928,#2935,#1865,.T.);
#3738=EDGE_CURVE('',#2933,#2927,#1866,.T.);
#3739=EDGE_CURVE('',#2887,#2934,#343,.T.);
#3740=EDGE_CURVE('',#2935,#2888,#344,.T.);
#3741=EDGE_CURVE('',#2936,#2937,#2519,.F.);
#3742=EDGE_CURVE('',#2938,#2936,#2520,.F.);
#3743=EDGE_CURVE('',#2937,#2938,#2521,.F.);
#3744=EDGE_CURVE('',#2936,#2932,#1867,.T.);
#3745=EDGE_CURVE('',#2930,#2938,#1868,.T.);
#3746=EDGE_CURVE('',#2934,#2937,#345,.T.);
#3747=EDGE_CURVE('',#2938,#2933,#346,.T.);
#3748=EDGE_CURVE('',#2885,#2936,#347,.T.);
#3749=EDGE_CURVE('',#2937,#2886,#348,.T.);
#3750=EDGE_CURVE('',#2883,#2931,#349,.T.);
#3751=EDGE_CURVE('',#2932,#2884,#350,.T.);
#3752=EDGE_CURVE('',#2931,#2929,#351,.T.);
#3753=EDGE_CURVE('',#2927,#2930,#352,.T.);
#3754=EDGE_CURVE('',#2881,#2928,#353,.T.);
#3755=EDGE_CURVE('',#2929,#2882,#354,.T.);
#3756=EDGE_CURVE('',#2939,#2939,#2522,.T.);
#3757=EDGE_CURVE('',#2939,#2940,#1869,.T.);
#3758=EDGE_CURVE('',#2940,#2940,#2523,.T.);
#3759=EDGE_CURVE('',#2941,#2941,#2524,.T.);
#3760=EDGE_CURVE('',#2941,#2942,#1870,.T.);
#3761=EDGE_CURVE('',#2942,#2942,#2525,.T.);
#3762=EDGE_CURVE('',#2943,#2943,#2526,.T.);
#3763=EDGE_CURVE('',#2944,#2944,#2527,.T.);
#3764=EDGE_CURVE('',#2945,#2945,#2528,.T.);
#3765=EDGE_CURVE('',#2945,#2943,#1871,.T.);
#3766=EDGE_CURVE('',#2946,#2946,#2529,.T.);
#3767=EDGE_CURVE('',#2947,#2947,#2530,.T.);
#3768=EDGE_CURVE('',#2948,#2948,#2531,.T.);
#3769=EDGE_CURVE('',#2948,#2946,#1872,.T.);
#3770=EDGE_CURVE('',#2949,#2949,#2532,.T.);
#3771=EDGE_CURVE('',#2950,#2950,#2533,.T.);
#3772=EDGE_CURVE('',#2951,#2951,#2534,.T.);
#3773=EDGE_CURVE('',#2951,#2949,#1873,.T.);
#3774=EDGE_CURVE('',#2952,#2952,#2535,.T.);
#3775=EDGE_CURVE('',#2953,#2953,#2536,.T.);
#3776=EDGE_CURVE('',#2954,#2954,#2537,.T.);
#3777=EDGE_CURVE('',#2954,#2952,#1874,.T.);
#3778=EDGE_CURVE('',#2944,#2955,#1875,.T.);
#3779=EDGE_CURVE('',#2955,#2955,#2538,.T.);
#3780=EDGE_CURVE('',#2947,#2956,#1876,.T.);
#3781=EDGE_CURVE('',#2956,#2956,#2539,.T.);
#3782=EDGE_CURVE('',#2950,#2957,#1877,.T.);
#3783=EDGE_CURVE('',#2957,#2957,#2540,.T.);
#3784=EDGE_CURVE('',#2953,#2958,#1878,.T.);
#3785=EDGE_CURVE('',#2958,#2958,#2541,.T.);
#3786=EDGE_CURVE('',#2959,#2960,#2542,.T.);
#3787=EDGE_CURVE('',#2960,#2961,#355,.T.);
#3788=EDGE_CURVE('',#2961,#2962,#2543,.T.);
#3789=EDGE_CURVE('',#2962,#2959,#356,.T.);
#3790=EDGE_CURVE('',#2963,#2964,#2544,.T.);
#3791=EDGE_CURVE('',#2964,#2960,#1879,.T.);
#3792=EDGE_CURVE('',#2959,#2963,#1880,.T.);
#3793=EDGE_CURVE('',#2965,#2966,#2545,.T.);
#3794=EDGE_CURVE('',#2966,#2964,#357,.T.);
#3795=EDGE_CURVE('',#2963,#2965,#358,.T.);
#3796=EDGE_CURVE('',#2967,#2968,#2546,.T.);
#3797=EDGE_CURVE('',#2968,#2966,#359,.T.);
#3798=EDGE_CURVE('',#2965,#2967,#360,.T.);
#3799=EDGE_CURVE('',#2969,#2970,#2547,.T.);
#3800=EDGE_CURVE('',#2970,#2968,#361,.T.);
#3801=EDGE_CURVE('',#2967,#2969,#362,.T.);
#3802=EDGE_CURVE('',#2971,#2972,#2548,.T.);
#3803=EDGE_CURVE('',#2972,#2970,#1881,.T.);
#3804=EDGE_CURVE('',#2969,#2971,#1882,.T.);
#3805=EDGE_CURVE('',#2973,#2974,#2549,.T.);
#3806=EDGE_CURVE('',#2974,#2972,#363,.T.);
#3807=EDGE_CURVE('',#2971,#2973,#364,.T.);
#3808=EDGE_CURVE('',#2961,#2974,#365,.T.);
#3809=EDGE_CURVE('',#2973,#2962,#366,.T.);
#3810=EDGE_CURVE('',#2975,#2972,#367,.T.);
#3811=EDGE_CURVE('',#2976,#2975,#1883,.T.);
#3812=EDGE_CURVE('',#2970,#2976,#368,.T.);
#3813=EDGE_CURVE('',#2974,#2977,#369,.T.);
#3814=EDGE_CURVE('',#2977,#2975,#370,.T.);
#3815=EDGE_CURVE('',#2978,#2961,#371,.T.);
#3816=EDGE_CURVE('',#2977,#2978,#372,.T.);
#3817=EDGE_CURVE('',#2960,#2979,#373,.T.);
#3818=EDGE_CURVE('',#2979,#2978,#374,.T.);
#3819=EDGE_CURVE('',#2980,#2964,#375,.T.);
#3820=EDGE_CURVE('',#2979,#2980,#1884,.T.);
#3821=EDGE_CURVE('',#2976,#2981,#376,.T.);
#3822=EDGE_CURVE('',#2981,#2968,#377,.T.);
#3823=EDGE_CURVE('',#2966,#2982,#378,.T.);
#3824=EDGE_CURVE('',#2982,#2980,#379,.T.);
#3825=EDGE_CURVE('',#2982,#2981,#380,.T.);
#3826=EDGE_CURVE('',#2983,#2984,#1885,.T.);
#3827=EDGE_CURVE('',#2983,#2985,#381,.T.);
#3828=EDGE_CURVE('',#2985,#2986,#2550,.F.);
#3829=EDGE_CURVE('',#2986,#2984,#382,.T.);
#3830=EDGE_CURVE('',#2987,#2988,#1886,.T.);
#3831=EDGE_CURVE('',#2987,#2983,#383,.T.);
#3832=EDGE_CURVE('',#2984,#2988,#384,.T.);
#3833=EDGE_CURVE('',#2989,#2990,#1887,.T.);
#3834=EDGE_CURVE('',#2989,#2987,#385,.T.);
#3835=EDGE_CURVE('',#2988,#2990,#386,.T.);
#3836=EDGE_CURVE('',#2991,#2992,#1888,.T.);
#3837=EDGE_CURVE('',#2991,#2989,#387,.T.);
#3838=EDGE_CURVE('',#2990,#2992,#388,.T.);
#3839=EDGE_CURVE('',#2993,#2994,#1889,.T.);
#3840=EDGE_CURVE('',#2993,#2991,#389,.T.);
#3841=EDGE_CURVE('',#2992,#2994,#390,.T.);
#3842=EDGE_CURVE('',#2995,#2996,#1890,.T.);
#3843=EDGE_CURVE('',#2995,#2993,#391,.T.);
#3844=EDGE_CURVE('',#2994,#2996,#392,.T.);
#3845=EDGE_CURVE('',#2997,#2998,#1891,.T.);
#3846=EDGE_CURVE('',#2997,#2995,#393,.T.);
#3847=EDGE_CURVE('',#2996,#2998,#394,.T.);
#3848=EDGE_CURVE('',#2999,#3000,#1892,.T.);
#3849=EDGE_CURVE('',#2999,#2997,#395,.T.);
#3850=EDGE_CURVE('',#2998,#3000,#396,.T.);
#3851=EDGE_CURVE('',#3001,#3002,#1893,.T.);
#3852=EDGE_CURVE('',#3001,#2999,#397,.T.);
#3853=EDGE_CURVE('',#3000,#3002,#398,.T.);
#3854=EDGE_CURVE('',#3003,#3004,#1894,.T.);
#3855=EDGE_CURVE('',#3003,#3001,#399,.T.);
#3856=EDGE_CURVE('',#3002,#3004,#400,.T.);
#3857=EDGE_CURVE('',#3005,#3006,#1895,.T.);
#3858=EDGE_CURVE('',#3005,#3003,#401,.T.);
#3859=EDGE_CURVE('',#3004,#3006,#402,.T.);
#3860=EDGE_CURVE('',#3007,#3008,#1896,.T.);
#3861=EDGE_CURVE('',#3007,#3005,#403,.T.);
#3862=EDGE_CURVE('',#3006,#3008,#404,.T.);
#3863=EDGE_CURVE('',#3009,#3010,#1897,.T.);
#3864=EDGE_CURVE('',#3009,#3007,#405,.T.);
#3865=EDGE_CURVE('',#3008,#3010,#406,.T.);
#3866=EDGE_CURVE('',#3011,#3012,#1898,.T.);
#3867=EDGE_CURVE('',#3011,#3009,#407,.T.);
#3868=EDGE_CURVE('',#3010,#3012,#408,.T.);
#3869=EDGE_CURVE('',#3013,#3014,#1899,.T.);
#3870=EDGE_CURVE('',#3013,#3011,#409,.T.);
#3871=EDGE_CURVE('',#3012,#3014,#410,.T.);
#3872=EDGE_CURVE('',#3015,#3016,#1900,.T.);
#3873=EDGE_CURVE('',#3015,#3013,#411,.T.);
#3874=EDGE_CURVE('',#3014,#3016,#412,.T.);
#3875=EDGE_CURVE('',#3017,#3018,#1901,.T.);
#3876=EDGE_CURVE('',#3017,#3015,#413,.T.);
#3877=EDGE_CURVE('',#3016,#3018,#414,.T.);
#3878=EDGE_CURVE('',#3019,#3020,#1902,.T.);
#3879=EDGE_CURVE('',#3019,#3017,#415,.T.);
#3880=EDGE_CURVE('',#3018,#3020,#416,.T.);
#3881=EDGE_CURVE('',#3021,#3022,#1903,.T.);
#3882=EDGE_CURVE('',#3021,#3019,#417,.T.);
#3883=EDGE_CURVE('',#3020,#3022,#418,.T.);
#3884=EDGE_CURVE('',#3023,#3024,#1904,.T.);
#3885=EDGE_CURVE('',#3023,#3021,#419,.T.);
#3886=EDGE_CURVE('',#3022,#3024,#420,.T.);
#3887=EDGE_CURVE('',#3025,#3026,#1905,.T.);
#3888=EDGE_CURVE('',#3025,#3023,#421,.T.);
#3889=EDGE_CURVE('',#3024,#3026,#422,.T.);
#3890=EDGE_CURVE('',#3027,#3028,#1906,.T.);
#3891=EDGE_CURVE('',#3027,#3025,#423,.T.);
#3892=EDGE_CURVE('',#3026,#3028,#424,.T.);
#3893=EDGE_CURVE('',#3029,#3030,#1907,.T.);
#3894=EDGE_CURVE('',#3029,#3027,#425,.T.);
#3895=EDGE_CURVE('',#3028,#3030,#426,.T.);
#3896=EDGE_CURVE('',#3031,#3032,#1908,.T.);
#3897=EDGE_CURVE('',#3031,#3029,#427,.T.);
#3898=EDGE_CURVE('',#3030,#3032,#428,.T.);
#3899=EDGE_CURVE('',#3033,#3034,#1909,.T.);
#3900=EDGE_CURVE('',#3033,#3031,#429,.T.);
#3901=EDGE_CURVE('',#3032,#3034,#430,.T.);
#3902=EDGE_CURVE('',#3035,#3036,#1910,.T.);
#3903=EDGE_CURVE('',#3035,#3033,#431,.T.);
#3904=EDGE_CURVE('',#3034,#3036,#432,.T.);
#3905=EDGE_CURVE('',#3037,#3038,#1911,.T.);
#3906=EDGE_CURVE('',#3037,#3035,#433,.T.);
#3907=EDGE_CURVE('',#3036,#3038,#434,.T.);
#3908=EDGE_CURVE('',#3039,#3040,#1912,.T.);
#3909=EDGE_CURVE('',#3039,#3037,#435,.T.);
#3910=EDGE_CURVE('',#3038,#3040,#436,.T.);
#3911=EDGE_CURVE('',#3041,#3042,#1913,.T.);
#3912=EDGE_CURVE('',#3041,#3039,#437,.T.);
#3913=EDGE_CURVE('',#3040,#3042,#438,.T.);
#3914=EDGE_CURVE('',#3043,#3044,#1914,.T.);
#3915=EDGE_CURVE('',#3043,#3041,#439,.T.);
#3916=EDGE_CURVE('',#3042,#3044,#440,.T.);
#3917=EDGE_CURVE('',#3045,#3046,#1915,.T.);
#3918=EDGE_CURVE('',#3045,#3047,#441,.T.);
#3919=EDGE_CURVE('',#3047,#3048,#2551,.T.);
#3920=EDGE_CURVE('',#3046,#3048,#442,.T.);
#3921=EDGE_CURVE('',#3049,#3050,#1916,.T.);
#3922=EDGE_CURVE('',#3049,#3045,#443,.T.);
#3923=EDGE_CURVE('',#3050,#3046,#444,.T.);
#3924=EDGE_CURVE('',#3051,#3052,#1917,.T.);
#3925=EDGE_CURVE('',#3051,#3049,#445,.T.);
#3926=EDGE_CURVE('',#3052,#3050,#446,.T.);
#3927=EDGE_CURVE('',#3053,#3054,#1918,.T.);
#3928=EDGE_CURVE('',#3053,#3051,#447,.T.);
#3929=EDGE_CURVE('',#3054,#3052,#448,.T.);
#3930=EDGE_CURVE('',#3055,#3056,#1919,.T.);
#3931=EDGE_CURVE('',#3055,#3053,#449,.T.);
#3932=EDGE_CURVE('',#3056,#3054,#450,.T.);
#3933=EDGE_CURVE('',#3057,#3058,#1920,.T.);
#3934=EDGE_CURVE('',#3057,#3055,#451,.T.);
#3935=EDGE_CURVE('',#3058,#3056,#452,.T.);
#3936=EDGE_CURVE('',#3059,#3060,#1921,.T.);
#3937=EDGE_CURVE('',#3059,#3057,#453,.T.);
#3938=EDGE_CURVE('',#3060,#3058,#454,.T.);
#3939=EDGE_CURVE('',#3061,#3062,#1922,.T.);
#3940=EDGE_CURVE('',#3061,#3059,#455,.T.);
#3941=EDGE_CURVE('',#3062,#3060,#456,.T.);
#3942=EDGE_CURVE('',#3063,#3064,#1923,.T.);
#3943=EDGE_CURVE('',#3063,#3061,#457,.T.);
#3944=EDGE_CURVE('',#3064,#3062,#458,.T.);
#3945=EDGE_CURVE('',#3065,#3066,#1924,.T.);
#3946=EDGE_CURVE('',#3065,#3063,#459,.T.);
#3947=EDGE_CURVE('',#3066,#3064,#460,.T.);
#3948=EDGE_CURVE('',#3067,#3068,#1925,.T.);
#3949=EDGE_CURVE('',#3067,#3065,#461,.T.);
#3950=EDGE_CURVE('',#3068,#3066,#462,.T.);
#3951=EDGE_CURVE('',#3069,#3070,#1926,.T.);
#3952=EDGE_CURVE('',#3069,#3067,#463,.T.);
#3953=EDGE_CURVE('',#3070,#3068,#464,.T.);
#3954=EDGE_CURVE('',#3071,#3072,#1927,.T.);
#3955=EDGE_CURVE('',#3071,#3069,#465,.T.);
#3956=EDGE_CURVE('',#3072,#3070,#466,.T.);
#3957=EDGE_CURVE('',#3073,#3074,#1928,.T.);
#3958=EDGE_CURVE('',#3073,#3071,#467,.T.);
#3959=EDGE_CURVE('',#3074,#3072,#468,.T.);
#3960=EDGE_CURVE('',#3075,#3076,#1929,.T.);
#3961=EDGE_CURVE('',#3075,#3073,#469,.T.);
#3962=EDGE_CURVE('',#3076,#3074,#470,.T.);
#3963=EDGE_CURVE('',#3077,#3078,#1930,.T.);
#3964=EDGE_CURVE('',#3077,#3075,#471,.T.);
#3965=EDGE_CURVE('',#3078,#3076,#472,.T.);
#3966=EDGE_CURVE('',#3079,#3080,#1931,.T.);
#3967=EDGE_CURVE('',#3079,#3077,#473,.T.);
#3968=EDGE_CURVE('',#3080,#3078,#474,.T.);
#3969=EDGE_CURVE('',#3081,#3082,#1932,.T.);
#3970=EDGE_CURVE('',#3081,#3079,#475,.T.);
#3971=EDGE_CURVE('',#3082,#3080,#476,.T.);
#3972=EDGE_CURVE('',#3083,#3084,#1933,.T.);
#3973=EDGE_CURVE('',#3083,#3081,#477,.T.);
#3974=EDGE_CURVE('',#3084,#3082,#478,.T.);
#3975=EDGE_CURVE('',#3085,#3086,#1934,.T.);
#3976=EDGE_CURVE('',#3085,#3083,#479,.T.);
#3977=EDGE_CURVE('',#3086,#3084,#480,.T.);
#3978=EDGE_CURVE('',#3087,#3088,#1935,.T.);
#3979=EDGE_CURVE('',#3087,#3085,#481,.T.);
#3980=EDGE_CURVE('',#3088,#3086,#482,.T.);
#3981=EDGE_CURVE('',#3089,#3090,#1936,.T.);
#3982=EDGE_CURVE('',#3089,#3087,#483,.T.);
#3983=EDGE_CURVE('',#3090,#3088,#484,.T.);
#3984=EDGE_CURVE('',#3091,#3092,#1937,.T.);
#3985=EDGE_CURVE('',#3091,#3089,#485,.T.);
#3986=EDGE_CURVE('',#3092,#3090,#486,.T.);
#3987=EDGE_CURVE('',#3093,#3094,#1938,.T.);
#3988=EDGE_CURVE('',#3093,#3091,#487,.T.);
#3989=EDGE_CURVE('',#3094,#3092,#488,.T.);
#3990=EDGE_CURVE('',#3095,#3096,#1939,.T.);
#3991=EDGE_CURVE('',#3095,#3093,#489,.T.);
#3992=EDGE_CURVE('',#3096,#3094,#490,.T.);
#3993=EDGE_CURVE('',#3097,#3098,#1940,.T.);
#3994=EDGE_CURVE('',#3097,#3095,#491,.T.);
#3995=EDGE_CURVE('',#3098,#3096,#492,.T.);
#3996=EDGE_CURVE('',#3099,#3100,#1941,.T.);
#3997=EDGE_CURVE('',#3099,#3097,#493,.T.);
#3998=EDGE_CURVE('',#3100,#3098,#494,.T.);
#3999=EDGE_CURVE('',#3101,#3102,#1942,.T.);
#4000=EDGE_CURVE('',#3101,#3099,#495,.T.);
#4001=EDGE_CURVE('',#3102,#3100,#496,.T.);
#4002=EDGE_CURVE('',#3103,#3104,#1943,.T.);
#4003=EDGE_CURVE('',#3103,#3101,#497,.T.);
#4004=EDGE_CURVE('',#3104,#3102,#498,.T.);
#4005=EDGE_CURVE('',#3105,#3106,#1944,.T.);
#4006=EDGE_CURVE('',#3105,#3103,#499,.T.);
#4007=EDGE_CURVE('',#3106,#3104,#500,.T.);
#4008=EDGE_CURVE('',#3048,#3107,#501,.T.);
#4009=EDGE_CURVE('',#3108,#3047,#502,.T.);
#4010=EDGE_CURVE('',#3109,#3108,#2552,.T.);
#4011=EDGE_CURVE('',#3107,#3109,#503,.T.);
#4012=EDGE_CURVE('',#3107,#3110,#1945,.T.);
#4013=EDGE_CURVE('',#3110,#3110,#2553,.T.);
#4014=EDGE_CURVE('',#3111,#3105,#504,.T.);
#4015=EDGE_CURVE('',#2985,#3111,#505,.T.);
#4016=EDGE_CURVE('',#3108,#3043,#506,.T.);
#4017=EDGE_CURVE('',#3112,#3106,#507,.T.);
#4018=EDGE_CURVE('',#3111,#3112,#2554,.T.);
#4019=EDGE_CURVE('',#3044,#3109,#508,.T.);
#4020=EDGE_CURVE('',#3112,#2986,#509,.T.);
#4021=EDGE_CURVE('',#3113,#3114,#1946,.T.);
#4022=EDGE_CURVE('',#3113,#3115,#1947,.T.);
#4023=EDGE_CURVE('',#3115,#3116,#1948,.T.);
#4024=EDGE_CURVE('',#3114,#3116,#1949,.T.);
#4025=EDGE_CURVE('',#3117,#3113,#1950,.T.);
#4026=EDGE_CURVE('',#3117,#3118,#1951,.T.);
#4027=EDGE_CURVE('',#3118,#3115,#1952,.T.);
#4028=EDGE_CURVE('',#3119,#3117,#1953,.T.);
#4029=EDGE_CURVE('',#3119,#3120,#1954,.T.);
#4030=EDGE_CURVE('',#3120,#3118,#1955,.T.);
#4031=EDGE_CURVE('',#3121,#3119,#1956,.T.);
#4032=EDGE_CURVE('',#3121,#3122,#1957,.T.);
#4033=EDGE_CURVE('',#3122,#3120,#1958,.T.);
#4034=EDGE_CURVE('',#3123,#3121,#1959,.T.);
#4035=EDGE_CURVE('',#3123,#3124,#1960,.T.);
#4036=EDGE_CURVE('',#3124,#3122,#1961,.T.);
#4037=EDGE_CURVE('',#3114,#3123,#1962,.T.);
#4038=EDGE_CURVE('',#3116,#3124,#1963,.T.);
#4039=EDGE_CURVE('',#3125,#3125,#2555,.T.);
#4040=EDGE_CURVE('',#3125,#3126,#1964,.T.);
#4041=EDGE_CURVE('',#3126,#3126,#2556,.T.);
#4042=EDGE_CURVE('',#3127,#3128,#1965,.T.);
#4043=EDGE_CURVE('',#3129,#3128,#2557,.F.);
#4044=EDGE_CURVE('',#3129,#3127,#510,.T.);
#4045=EDGE_CURVE('',#3130,#3131,#1966,.T.);
#4046=EDGE_CURVE('',#3131,#3132,#511,.T.);
#4047=EDGE_CURVE('',#3128,#3132,#2558,.F.);
#4048=EDGE_CURVE('',#3127,#3130,#512,.T.);
#4049=EDGE_CURVE('',#3133,#3134,#1967,.T.);
#4050=EDGE_CURVE('',#3134,#3131,#513,.T.);
#4051=EDGE_CURVE('',#3130,#3133,#514,.T.);
#4052=EDGE_CURVE('',#3135,#3136,#1968,.T.);
#4053=EDGE_CURVE('',#3136,#3134,#515,.T.);
#4054=EDGE_CURVE('',#3133,#3135,#516,.T.);
#4055=EDGE_CURVE('',#3137,#3138,#1969,.T.);
#4056=EDGE_CURVE('',#3137,#3139,#517,.T.);
#4057=EDGE_CURVE('',#3140,#3139,#2559,.T.);
#4058=EDGE_CURVE('',#3140,#3138,#518,.T.);
#4059=EDGE_CURVE('',#3141,#3142,#1970,.T.);
#4060=EDGE_CURVE('',#3142,#3143,#519,.T.);
#4061=EDGE_CURVE('',#3144,#3143,#2560,.T.);
#4062=EDGE_CURVE('',#3141,#3144,#520,.T.);
#4063=EDGE_CURVE('',#3145,#3146,#1971,.T.);
#4064=EDGE_CURVE('',#3146,#3142,#521,.T.);
#4065=EDGE_CURVE('',#3145,#3141,#522,.T.);
#4066=EDGE_CURVE('',#3147,#3148,#1972,.T.);
#4067=EDGE_CURVE('',#3148,#3146,#523,.T.);
#4068=EDGE_CURVE('',#3147,#3145,#524,.T.);
#4069=EDGE_CURVE('',#3149,#3150,#1973,.T.);
#4070=EDGE_CURVE('',#3150,#3148,#525,.T.);
#4071=EDGE_CURVE('',#3149,#3147,#526,.T.);
#4072=EDGE_CURVE('',#3151,#3152,#1974,.T.);
#4073=EDGE_CURVE('',#3153,#3151,#527,.T.);
#4074=EDGE_CURVE('',#3154,#3153,#2561,.T.);
#4075=EDGE_CURVE('',#3154,#3152,#528,.T.);
#4076=EDGE_CURVE('',#3152,#3150,#529,.T.);
#4077=EDGE_CURVE('',#3151,#3149,#530,.T.);
#4078=EDGE_CURVE('',#3143,#3129,#531,.T.);
#4079=EDGE_CURVE('',#3139,#3154,#532,.T.);
#4080=EDGE_CURVE('',#3135,#3137,#533,.T.);
#4081=EDGE_CURVE('',#3132,#3144,#534,.T.);
#4082=EDGE_CURVE('',#3138,#3136,#535,.T.);
#4083=EDGE_CURVE('',#3153,#3140,#536,.T.);
#4084=EDGE_CURVE('',#3155,#3156,#1975,.T.);
#4085=EDGE_CURVE('',#3156,#3157,#1976,.T.);
#4086=EDGE_CURVE('',#3157,#3158,#1977,.T.);
#4087=EDGE_CURVE('',#3158,#3159,#1978,.T.);
#4088=EDGE_CURVE('',#3159,#3160,#1979,.T.);
#4089=EDGE_CURVE('',#3160,#3155,#1980,.T.);
#4090=EDGE_CURVE('',#3161,#3162,#1981,.T.);
#4091=EDGE_CURVE('',#3162,#3155,#1982,.T.);
#4092=EDGE_CURVE('',#3161,#3160,#1983,.T.);
#4093=EDGE_CURVE('',#3163,#3161,#1984,.T.);
#4094=EDGE_CURVE('',#3163,#3159,#1985,.T.);
#4095=EDGE_CURVE('',#3164,#3163,#1986,.T.);
#4096=EDGE_CURVE('',#3164,#3158,#1987,.T.);
#4097=EDGE_CURVE('',#3165,#3164,#1988,.T.);
#4098=EDGE_CURVE('',#3165,#3157,#1989,.T.);
#4099=EDGE_CURVE('',#3166,#3165,#1990,.T.);
#4100=EDGE_CURVE('',#3166,#3156,#1991,.T.);
#4101=EDGE_CURVE('',#3162,#3166,#1992,.T.);
#4102=EDGE_CURVE('',#3167,#3167,#2562,.T.);
#4103=EDGE_CURVE('',#3167,#3168,#1993,.T.);
#4104=EDGE_CURVE('',#3168,#3168,#2563,.T.);
#4105=EDGE_CURVE('',#3169,#3169,#2564,.T.);
#4106=EDGE_CURVE('',#3169,#3170,#1994,.T.);
#4107=EDGE_CURVE('',#3170,#3170,#2565,.T.);
#4108=ORIENTED_EDGE('',*,*,#3171,.F.);
#4109=ORIENTED_EDGE('',*,*,#3172,.T.);
#4110=ORIENTED_EDGE('',*,*,#3173,.F.);
#4111=ORIENTED_EDGE('',*,*,#3172,.F.);
#4112=ORIENTED_EDGE('',*,*,#3174,.F.);
#4113=ORIENTED_EDGE('',*,*,#3175,.T.);
#4114=ORIENTED_EDGE('',*,*,#3176,.F.);
#4115=ORIENTED_EDGE('',*,*,#3175,.F.);
#4116=ORIENTED_EDGE('',*,*,#3177,.F.);
#4117=ORIENTED_EDGE('',*,*,#3178,.T.);
#4118=ORIENTED_EDGE('',*,*,#3179,.F.);
#4119=ORIENTED_EDGE('',*,*,#3178,.F.);
#4120=ORIENTED_EDGE('',*,*,#3180,.F.);
#4121=ORIENTED_EDGE('',*,*,#3181,.F.);
#4122=ORIENTED_EDGE('',*,*,#3182,.T.);
#4123=ORIENTED_EDGE('',*,*,#3183,.F.);
#4124=ORIENTED_EDGE('',*,*,#3184,.T.);
#4125=ORIENTED_EDGE('',*,*,#3181,.T.);
#4126=ORIENTED_EDGE('',*,*,#3185,.F.);
#4127=ORIENTED_EDGE('',*,*,#3186,.F.);
#4128=ORIENTED_EDGE('',*,*,#3187,.F.);
#4129=ORIENTED_EDGE('',*,*,#3183,.T.);
#4130=ORIENTED_EDGE('',*,*,#3188,.F.);
#4131=ORIENTED_EDGE('',*,*,#3189,.F.);
#4132=ORIENTED_EDGE('',*,*,#3182,.F.);
#4133=ORIENTED_EDGE('',*,*,#3190,.F.);
#4134=ORIENTED_EDGE('',*,*,#3191,.F.);
#4135=ORIENTED_EDGE('',*,*,#3192,.T.);
#4136=ORIENTED_EDGE('',*,*,#3193,.F.);
#4137=ORIENTED_EDGE('',*,*,#3194,.F.);
#4138=ORIENTED_EDGE('',*,*,#3195,.T.);
#4139=ORIENTED_EDGE('',*,*,#3187,.T.);
#4140=ORIENTED_EDGE('',*,*,#3196,.F.);
#4141=ORIENTED_EDGE('',*,*,#3197,.F.);
#4142=ORIENTED_EDGE('',*,*,#3198,.T.);
#4143=ORIENTED_EDGE('',*,*,#3197,.T.);
#4144=ORIENTED_EDGE('',*,*,#3199,.F.);
#4145=ORIENTED_EDGE('',*,*,#3192,.F.);
#4146=ORIENTED_EDGE('',*,*,#3180,.T.);
#4147=ORIENTED_EDGE('',*,*,#3189,.T.);
#4148=ORIENTED_EDGE('',*,*,#3200,.F.);
#4149=ORIENTED_EDGE('',*,*,#3201,.F.);
#4150=ORIENTED_EDGE('',*,*,#3193,.T.);
#4151=ORIENTED_EDGE('',*,*,#3199,.T.);
#4152=ORIENTED_EDGE('',*,*,#3196,.T.);
#4153=ORIENTED_EDGE('',*,*,#3186,.T.);
#4154=ORIENTED_EDGE('',*,*,#3185,.T.);
#4155=ORIENTED_EDGE('',*,*,#3194,.T.);
#4156=ORIENTED_EDGE('',*,*,#3201,.T.);
#4157=ORIENTED_EDGE('',*,*,#3202,.T.);
#4158=ORIENTED_EDGE('',*,*,#3203,.F.);
#4159=ORIENTED_EDGE('',*,*,#3204,.F.);
#4160=ORIENTED_EDGE('',*,*,#3205,.F.);
#4161=ORIENTED_EDGE('',*,*,#3200,.T.);
#4162=ORIENTED_EDGE('',*,*,#3188,.T.);
#4163=ORIENTED_EDGE('',*,*,#3206,.F.);
#4164=ORIENTED_EDGE('',*,*,#3207,.T.);
#4165=ORIENTED_EDGE('',*,*,#3208,.F.);
#4166=ORIENTED_EDGE('',*,*,#3202,.F.);
#4167=ORIENTED_EDGE('',*,*,#3209,.F.);
#4168=ORIENTED_EDGE('',*,*,#3210,.F.);
#4169=ORIENTED_EDGE('',*,*,#3207,.F.);
#4170=ORIENTED_EDGE('',*,*,#3211,.F.);
#4171=ORIENTED_EDGE('',*,*,#3212,.F.);
#4172=ORIENTED_EDGE('',*,*,#3213,.F.);
#4173=ORIENTED_EDGE('',*,*,#3204,.T.);
#4174=ORIENTED_EDGE('',*,*,#3214,.F.);
#4175=ORIENTED_EDGE('',*,*,#3209,.T.);
#4176=ORIENTED_EDGE('',*,*,#3215,.T.);
#4177=ORIENTED_EDGE('',*,*,#3216,.T.);
#4178=ORIENTED_EDGE('',*,*,#3217,.F.);
#4179=ORIENTED_EDGE('',*,*,#3212,.T.);
#4180=ORIENTED_EDGE('',*,*,#3218,.F.);
#4181=ORIENTED_EDGE('',*,*,#3219,.T.);
#4182=ORIENTED_EDGE('',*,*,#3220,.T.);
#4183=ORIENTED_EDGE('',*,*,#3217,.T.);
#4184=ORIENTED_EDGE('',*,*,#3221,.T.);
#4185=ORIENTED_EDGE('',*,*,#3222,.T.);
#4186=ORIENTED_EDGE('',*,*,#3223,.T.);
#4187=ORIENTED_EDGE('',*,*,#3224,.T.);
#4188=ORIENTED_EDGE('',*,*,#3225,.T.);
#4189=ORIENTED_EDGE('',*,*,#3226,.T.);
#4190=ORIENTED_EDGE('',*,*,#3227,.T.);
#4191=ORIENTED_EDGE('',*,*,#3228,.T.);
#4192=ORIENTED_EDGE('',*,*,#3229,.T.);
#4193=ORIENTED_EDGE('',*,*,#3230,.T.);
#4194=ORIENTED_EDGE('',*,*,#3218,.T.);
#4195=ORIENTED_EDGE('',*,*,#3214,.T.);
#4196=ORIENTED_EDGE('',*,*,#3203,.T.);
#4197=ORIENTED_EDGE('',*,*,#3208,.T.);
#4198=ORIENTED_EDGE('',*,*,#3210,.T.);
#4199=ORIENTED_EDGE('',*,*,#3171,.T.);
#4200=ORIENTED_EDGE('',*,*,#3174,.T.);
#4201=ORIENTED_EDGE('',*,*,#3177,.T.);
#4202=ORIENTED_EDGE('',*,*,#3231,.F.);
#4203=ORIENTED_EDGE('',*,*,#3232,.T.);
#4204=ORIENTED_EDGE('',*,*,#3233,.T.);
#4205=ORIENTED_EDGE('',*,*,#3234,.T.);
#4206=ORIENTED_EDGE('',*,*,#3233,.F.);
#4207=ORIENTED_EDGE('',*,*,#3235,.F.);
#4208=ORIENTED_EDGE('',*,*,#3236,.F.);
#4209=ORIENTED_EDGE('',*,*,#3237,.T.);
#4210=ORIENTED_EDGE('',*,*,#3234,.F.);
#4211=ORIENTED_EDGE('',*,*,#3237,.F.);
#4212=ORIENTED_EDGE('',*,*,#3205,.T.);
#4213=ORIENTED_EDGE('',*,*,#3213,.T.);
#4214=ORIENTED_EDGE('',*,*,#3220,.F.);
#4215=ORIENTED_EDGE('',*,*,#3238,.F.);
#4216=ORIENTED_EDGE('',*,*,#3239,.F.);
#4217=ORIENTED_EDGE('',*,*,#3240,.F.);
#4218=ORIENTED_EDGE('',*,*,#3241,.F.);
#4219=ORIENTED_EDGE('',*,*,#3242,.F.);
#4220=ORIENTED_EDGE('',*,*,#3243,.F.);
#4221=ORIENTED_EDGE('',*,*,#3244,.F.);
#4222=ORIENTED_EDGE('',*,*,#3245,.F.);
#4223=ORIENTED_EDGE('',*,*,#3246,.F.);
#4224=ORIENTED_EDGE('',*,*,#3247,.F.);
#4225=ORIENTED_EDGE('',*,*,#3215,.F.);
#4226=ORIENTED_EDGE('',*,*,#3211,.T.);
#4227=ORIENTED_EDGE('',*,*,#3206,.T.);
#4228=ORIENTED_EDGE('',*,*,#3190,.T.);
#4229=ORIENTED_EDGE('',*,*,#3184,.F.);
#4230=ORIENTED_EDGE('',*,*,#3195,.F.);
#4231=ORIENTED_EDGE('',*,*,#3198,.F.);
#4232=ORIENTED_EDGE('',*,*,#3191,.T.);
#4233=ORIENTED_EDGE('',*,*,#3173,.T.);
#4234=ORIENTED_EDGE('',*,*,#3176,.T.);
#4235=ORIENTED_EDGE('',*,*,#3179,.T.);
#4236=ORIENTED_EDGE('',*,*,#3232,.F.);
#4237=ORIENTED_EDGE('',*,*,#3231,.T.);
#4238=ORIENTED_EDGE('',*,*,#3248,.T.);
#4239=ORIENTED_EDGE('',*,*,#3235,.T.);
#4240=ORIENTED_EDGE('',*,*,#3236,.T.);
#4241=ORIENTED_EDGE('',*,*,#3248,.F.);
#4242=ORIENTED_EDGE('',*,*,#3249,.F.);
#4243=ORIENTED_EDGE('',*,*,#3228,.F.);
#4244=ORIENTED_EDGE('',*,*,#3250,.F.);
#4245=ORIENTED_EDGE('',*,*,#3240,.T.);
#4246=ORIENTED_EDGE('',*,*,#3251,.F.);
#4247=ORIENTED_EDGE('',*,*,#3246,.T.);
#4248=ORIENTED_EDGE('',*,*,#3252,.F.);
#4249=ORIENTED_EDGE('',*,*,#3222,.F.);
#4250=ORIENTED_EDGE('',*,*,#3252,.T.);
#4251=ORIENTED_EDGE('',*,*,#3245,.T.);
#4252=ORIENTED_EDGE('',*,*,#3253,.T.);
#4253=ORIENTED_EDGE('',*,*,#3223,.F.);
#4254=ORIENTED_EDGE('',*,*,#3250,.T.);
#4255=ORIENTED_EDGE('',*,*,#3227,.F.);
#4256=ORIENTED_EDGE('',*,*,#3254,.F.);
#4257=ORIENTED_EDGE('',*,*,#3241,.T.);
#4258=ORIENTED_EDGE('',*,*,#3251,.T.);
#4259=ORIENTED_EDGE('',*,*,#3221,.F.);
#4260=ORIENTED_EDGE('',*,*,#3216,.F.);
#4261=ORIENTED_EDGE('',*,*,#3247,.T.);
#4262=ORIENTED_EDGE('',*,*,#3219,.F.);
#4263=ORIENTED_EDGE('',*,*,#3230,.F.);
#4264=ORIENTED_EDGE('',*,*,#3255,.F.);
#4265=ORIENTED_EDGE('',*,*,#3238,.T.);
#4266=ORIENTED_EDGE('',*,*,#3249,.T.);
#4267=ORIENTED_EDGE('',*,*,#3239,.T.);
#4268=ORIENTED_EDGE('',*,*,#3255,.T.);
#4269=ORIENTED_EDGE('',*,*,#3229,.F.);
#4270=ORIENTED_EDGE('',*,*,#3242,.T.);
#4271=ORIENTED_EDGE('',*,*,#3254,.T.);
#4272=ORIENTED_EDGE('',*,*,#3226,.F.);
#4273=ORIENTED_EDGE('',*,*,#3256,.F.);
#4274=ORIENTED_EDGE('',*,*,#3243,.T.);
#4275=ORIENTED_EDGE('',*,*,#3256,.T.);
#4276=ORIENTED_EDGE('',*,*,#3225,.F.);
#4277=ORIENTED_EDGE('',*,*,#3257,.F.);
#4278=ORIENTED_EDGE('',*,*,#3244,.T.);
#4279=ORIENTED_EDGE('',*,*,#3257,.T.);
#4280=ORIENTED_EDGE('',*,*,#3224,.F.);
#4281=ORIENTED_EDGE('',*,*,#3253,.F.);
#4282=ORIENTED_EDGE('',*,*,#3258,.T.);
#4283=ORIENTED_EDGE('',*,*,#3259,.T.);
#4284=ORIENTED_EDGE('',*,*,#3260,.F.);
#4285=ORIENTED_EDGE('',*,*,#3259,.F.);
#4286=ORIENTED_EDGE('',*,*,#3261,.F.);
#4287=ORIENTED_EDGE('',*,*,#3258,.F.);
#4288=ORIENTED_EDGE('',*,*,#3262,.F.);
#4289=ORIENTED_EDGE('',*,*,#3260,.T.);
#4290=ORIENTED_EDGE('',*,*,#3263,.F.);
#4291=ORIENTED_EDGE('',*,*,#3264,.T.);
#4292=ORIENTED_EDGE('',*,*,#3262,.T.);
#4293=ORIENTED_EDGE('',*,*,#3264,.F.);
#4294=ORIENTED_EDGE('',*,*,#3265,.T.);
#4295=ORIENTED_EDGE('',*,*,#3266,.F.);
#4296=ORIENTED_EDGE('',*,*,#3265,.F.);
#4297=ORIENTED_EDGE('',*,*,#3267,.T.);
#4298=ORIENTED_EDGE('',*,*,#3268,.T.);
#4299=ORIENTED_EDGE('',*,*,#3267,.F.);
#4300=ORIENTED_EDGE('',*,*,#3268,.F.);
#4301=ORIENTED_EDGE('',*,*,#3261,.T.);
#4302=ORIENTED_EDGE('',*,*,#3269,.T.);
#4303=ORIENTED_EDGE('',*,*,#3266,.T.);
#4304=ORIENTED_EDGE('',*,*,#3269,.F.);
#4305=ORIENTED_EDGE('',*,*,#3263,.T.);
#4306=ORIENTED_EDGE('',*,*,#3270,.F.);
#4307=ORIENTED_EDGE('',*,*,#3271,.F.);
#4308=ORIENTED_EDGE('',*,*,#3272,.F.);
#4309=ORIENTED_EDGE('',*,*,#3273,.F.);
#4310=ORIENTED_EDGE('',*,*,#3274,.F.);
#4311=ORIENTED_EDGE('',*,*,#3275,.F.);
#4312=ORIENTED_EDGE('',*,*,#3276,.F.);
#4313=ORIENTED_EDGE('',*,*,#3277,.F.);
#4314=ORIENTED_EDGE('',*,*,#3277,.T.);
#4315=ORIENTED_EDGE('',*,*,#3278,.F.);
#4316=ORIENTED_EDGE('',*,*,#3271,.T.);
#4317=ORIENTED_EDGE('',*,*,#3279,.F.);
#4318=ORIENTED_EDGE('',*,*,#3274,.T.);
#4319=ORIENTED_EDGE('',*,*,#3279,.T.);
#4320=ORIENTED_EDGE('',*,*,#3270,.T.);
#4321=ORIENTED_EDGE('',*,*,#3280,.F.);
#4322=ORIENTED_EDGE('',*,*,#3276,.T.);
#4323=ORIENTED_EDGE('',*,*,#3281,.F.);
#4324=ORIENTED_EDGE('',*,*,#3272,.T.);
#4325=ORIENTED_EDGE('',*,*,#3278,.T.);
#4326=ORIENTED_EDGE('',*,*,#3275,.T.);
#4327=ORIENTED_EDGE('',*,*,#3280,.T.);
#4328=ORIENTED_EDGE('',*,*,#3273,.T.);
#4329=ORIENTED_EDGE('',*,*,#3281,.T.);
#4330=ORIENTED_EDGE('',*,*,#3282,.F.);
#4331=ORIENTED_EDGE('',*,*,#3283,.T.);
#4332=ORIENTED_EDGE('',*,*,#3284,.F.);
#4333=ORIENTED_EDGE('',*,*,#3283,.F.);
#4334=ORIENTED_EDGE('',*,*,#3285,.F.);
#4335=ORIENTED_EDGE('',*,*,#3286,.T.);
#4336=ORIENTED_EDGE('',*,*,#3287,.F.);
#4337=ORIENTED_EDGE('',*,*,#3286,.F.);
#4338=ORIENTED_EDGE('',*,*,#3288,.F.);
#4339=ORIENTED_EDGE('',*,*,#3289,.T.);
#4340=ORIENTED_EDGE('',*,*,#3290,.F.);
#4341=ORIENTED_EDGE('',*,*,#3289,.F.);
#4342=ORIENTED_EDGE('',*,*,#3291,.F.);
#4343=ORIENTED_EDGE('',*,*,#3292,.T.);
#4344=ORIENTED_EDGE('',*,*,#3293,.F.);
#4345=ORIENTED_EDGE('',*,*,#3292,.F.);
#4346=ORIENTED_EDGE('',*,*,#3294,.F.);
#4347=ORIENTED_EDGE('',*,*,#3295,.T.);
#4348=ORIENTED_EDGE('',*,*,#3296,.T.);
#4349=ORIENTED_EDGE('',*,*,#3295,.F.);
#4350=ORIENTED_EDGE('',*,*,#3296,.F.);
#4351=ORIENTED_EDGE('',*,*,#3297,.F.);
#4352=ORIENTED_EDGE('',*,*,#3298,.F.);
#4353=ORIENTED_EDGE('',*,*,#3299,.T.);
#4354=ORIENTED_EDGE('',*,*,#3300,.T.);
#4355=ORIENTED_EDGE('',*,*,#3299,.F.);
#4356=ORIENTED_EDGE('',*,*,#3300,.F.);
#4357=ORIENTED_EDGE('',*,*,#3301,.F.);
#4358=ORIENTED_EDGE('',*,*,#3297,.T.);
#4359=ORIENTED_EDGE('',*,*,#3302,.T.);
#4360=ORIENTED_EDGE('',*,*,#3303,.F.);
#4361=ORIENTED_EDGE('',*,*,#3302,.F.);
#4362=ORIENTED_EDGE('',*,*,#3301,.T.);
#4363=ORIENTED_EDGE('',*,*,#3304,.T.);
#4364=ORIENTED_EDGE('',*,*,#3305,.F.);
#4365=ORIENTED_EDGE('',*,*,#3304,.F.);
#4366=ORIENTED_EDGE('',*,*,#3306,.F.);
#4367=ORIENTED_EDGE('',*,*,#3307,.F.);
#4368=ORIENTED_EDGE('',*,*,#3308,.F.);
#4369=ORIENTED_EDGE('',*,*,#3309,.T.);
#4370=ORIENTED_EDGE('',*,*,#3310,.F.);
#4371=ORIENTED_EDGE('',*,*,#3311,.T.);
#4372=ORIENTED_EDGE('',*,*,#3312,.F.);
#4373=ORIENTED_EDGE('',*,*,#3313,.F.);
#4374=ORIENTED_EDGE('',*,*,#3314,.F.);
#4375=ORIENTED_EDGE('',*,*,#3315,.T.);
#4376=ORIENTED_EDGE('',*,*,#3316,.F.);
#4377=ORIENTED_EDGE('',*,*,#3317,.F.);
#4378=ORIENTED_EDGE('',*,*,#3318,.F.);
#4379=ORIENTED_EDGE('',*,*,#3319,.T.);
#4380=ORIENTED_EDGE('',*,*,#3320,.F.);
#4381=ORIENTED_EDGE('',*,*,#3321,.F.);
#4382=ORIENTED_EDGE('',*,*,#3322,.F.);
#4383=ORIENTED_EDGE('',*,*,#3323,.T.);
#4384=ORIENTED_EDGE('',*,*,#3324,.F.);
#4385=ORIENTED_EDGE('',*,*,#3325,.F.);
#4386=ORIENTED_EDGE('',*,*,#3326,.F.);
#4387=ORIENTED_EDGE('',*,*,#3327,.F.);
#4388=ORIENTED_EDGE('',*,*,#3328,.F.);
#4389=ORIENTED_EDGE('',*,*,#3329,.T.);
#4390=ORIENTED_EDGE('',*,*,#3330,.F.);
#4391=ORIENTED_EDGE('',*,*,#3331,.F.);
#4392=ORIENTED_EDGE('',*,*,#3332,.F.);
#4393=ORIENTED_EDGE('',*,*,#3333,.T.);
#4394=ORIENTED_EDGE('',*,*,#3334,.F.);
#4395=ORIENTED_EDGE('',*,*,#3303,.T.);
#4396=ORIENTED_EDGE('',*,*,#3335,.F.);
#4397=ORIENTED_EDGE('',*,*,#3305,.T.);
#4398=ORIENTED_EDGE('',*,*,#3336,.F.);
#4399=ORIENTED_EDGE('',*,*,#3309,.F.);
#4400=ORIENTED_EDGE('',*,*,#3337,.F.);
#4401=ORIENTED_EDGE('',*,*,#3323,.F.);
#4402=ORIENTED_EDGE('',*,*,#3338,.F.);
#4403=ORIENTED_EDGE('',*,*,#3329,.F.);
#4404=ORIENTED_EDGE('',*,*,#3339,.F.);
#4405=ORIENTED_EDGE('',*,*,#3311,.F.);
#4406=ORIENTED_EDGE('',*,*,#3340,.F.);
#4407=ORIENTED_EDGE('',*,*,#3333,.F.);
#4408=ORIENTED_EDGE('',*,*,#3341,.F.);
#4409=ORIENTED_EDGE('',*,*,#3315,.F.);
#4410=ORIENTED_EDGE('',*,*,#3342,.F.);
#4411=ORIENTED_EDGE('',*,*,#3343,.F.);
#4412=ORIENTED_EDGE('',*,*,#3344,.F.);
#4413=ORIENTED_EDGE('',*,*,#3319,.F.);
#4414=ORIENTED_EDGE('',*,*,#3345,.F.);
#4415=ORIENTED_EDGE('',*,*,#3346,.F.);
#4416=ORIENTED_EDGE('',*,*,#3347,.F.);
#4417=ORIENTED_EDGE('',*,*,#3343,.T.);
#4418=ORIENTED_EDGE('',*,*,#3348,.T.);
#4419=ORIENTED_EDGE('',*,*,#3349,.F.);
#4420=ORIENTED_EDGE('',*,*,#3350,.F.);
#4421=ORIENTED_EDGE('',*,*,#3351,.F.);
#4422=ORIENTED_EDGE('',*,*,#3352,.F.);
#4423=ORIENTED_EDGE('',*,*,#3353,.F.);
#4424=ORIENTED_EDGE('',*,*,#3320,.T.);
#4425=ORIENTED_EDGE('',*,*,#3344,.T.);
#4426=ORIENTED_EDGE('',*,*,#3347,.T.);
#4427=ORIENTED_EDGE('',*,*,#3354,.T.);
#4428=ORIENTED_EDGE('',*,*,#3355,.F.);
#4429=ORIENTED_EDGE('',*,*,#3356,.F.);
#4430=ORIENTED_EDGE('',*,*,#3357,.F.);
#4431=ORIENTED_EDGE('',*,*,#3358,.F.);
#4432=ORIENTED_EDGE('',*,*,#3359,.F.);
#4433=ORIENTED_EDGE('',*,*,#3360,.T.);
#4434=ORIENTED_EDGE('',*,*,#3316,.T.);
#4435=ORIENTED_EDGE('',*,*,#3341,.T.);
#4436=ORIENTED_EDGE('',*,*,#3332,.T.);
#4437=ORIENTED_EDGE('',*,*,#3361,.T.);
#4438=ORIENTED_EDGE('',*,*,#3362,.F.);
#4439=ORIENTED_EDGE('',*,*,#3363,.F.);
#4440=ORIENTED_EDGE('',*,*,#3364,.F.);
#4441=ORIENTED_EDGE('',*,*,#3365,.F.);
#4442=ORIENTED_EDGE('',*,*,#3366,.F.);
#4443=ORIENTED_EDGE('',*,*,#3367,.T.);
#4444=ORIENTED_EDGE('',*,*,#3312,.T.);
#4445=ORIENTED_EDGE('',*,*,#3339,.T.);
#4446=ORIENTED_EDGE('',*,*,#3328,.T.);
#4447=ORIENTED_EDGE('',*,*,#3368,.T.);
#4448=ORIENTED_EDGE('',*,*,#3369,.F.);
#4449=ORIENTED_EDGE('',*,*,#3370,.F.);
#4450=ORIENTED_EDGE('',*,*,#3371,.F.);
#4451=ORIENTED_EDGE('',*,*,#3372,.F.);
#4452=ORIENTED_EDGE('',*,*,#3373,.F.);
#4453=ORIENTED_EDGE('',*,*,#3374,.T.);
#4454=ORIENTED_EDGE('',*,*,#3306,.T.);
#4455=ORIENTED_EDGE('',*,*,#3336,.T.);
#4456=ORIENTED_EDGE('',*,*,#3322,.T.);
#4457=ORIENTED_EDGE('',*,*,#3375,.F.);
#4458=ORIENTED_EDGE('',*,*,#3376,.T.);
#4459=ORIENTED_EDGE('',*,*,#3377,.T.);
#4460=ORIENTED_EDGE('',*,*,#3378,.T.);
#4461=ORIENTED_EDGE('',*,*,#3379,.F.);
#4462=ORIENTED_EDGE('',*,*,#3321,.T.);
#4463=ORIENTED_EDGE('',*,*,#3360,.F.);
#4464=ORIENTED_EDGE('',*,*,#3380,.T.);
#4465=ORIENTED_EDGE('',*,*,#3348,.F.);
#4466=ORIENTED_EDGE('',*,*,#3381,.T.);
#4467=ORIENTED_EDGE('',*,*,#3354,.F.);
#4468=ORIENTED_EDGE('',*,*,#3346,.T.);
#4469=ORIENTED_EDGE('',*,*,#3382,.F.);
#4470=ORIENTED_EDGE('',*,*,#3383,.T.);
#4471=ORIENTED_EDGE('',*,*,#3361,.F.);
#4472=ORIENTED_EDGE('',*,*,#3331,.T.);
#4473=ORIENTED_EDGE('',*,*,#3384,.F.);
#4474=ORIENTED_EDGE('',*,*,#3385,.T.);
#4475=ORIENTED_EDGE('',*,*,#3368,.F.);
#4476=ORIENTED_EDGE('',*,*,#3327,.T.);
#4477=ORIENTED_EDGE('',*,*,#3386,.F.);
#4478=ORIENTED_EDGE('',*,*,#3387,.T.);
#4479=ORIENTED_EDGE('',*,*,#3388,.T.);
#4480=ORIENTED_EDGE('',*,*,#3375,.T.);
#4481=ORIENTED_EDGE('',*,*,#3325,.T.);
#4482=ORIENTED_EDGE('',*,*,#3389,.T.);
#4483=ORIENTED_EDGE('',*,*,#3390,.F.);
#4484=ORIENTED_EDGE('',*,*,#3391,.T.);
#4485=ORIENTED_EDGE('',*,*,#3392,.F.);
#4486=ORIENTED_EDGE('',*,*,#3393,.T.);
#4487=ORIENTED_EDGE('',*,*,#3394,.F.);
#4488=ORIENTED_EDGE('',*,*,#3395,.T.);
#4489=ORIENTED_EDGE('',*,*,#3396,.F.);
#4490=ORIENTED_EDGE('',*,*,#3397,.T.);
#4491=ORIENTED_EDGE('',*,*,#3307,.T.);
#4492=ORIENTED_EDGE('',*,*,#3379,.T.);
#4493=ORIENTED_EDGE('',*,*,#3398,.T.);
#4494=ORIENTED_EDGE('',*,*,#3399,.T.);
#4495=ORIENTED_EDGE('',*,*,#3400,.F.);
#4496=ORIENTED_EDGE('',*,*,#3313,.T.);
#4497=ORIENTED_EDGE('',*,*,#3374,.F.);
#4498=ORIENTED_EDGE('',*,*,#3401,.T.);
#4499=ORIENTED_EDGE('',*,*,#3402,.F.);
#4500=ORIENTED_EDGE('',*,*,#3317,.T.);
#4501=ORIENTED_EDGE('',*,*,#3367,.F.);
#4502=ORIENTED_EDGE('',*,*,#3403,.T.);
#4503=ORIENTED_EDGE('',*,*,#3404,.F.);
#4504=ORIENTED_EDGE('',*,*,#3405,.T.);
#4505=ORIENTED_EDGE('',*,*,#3406,.T.);
#4506=ORIENTED_EDGE('',*,*,#3407,.T.);
#4507=ORIENTED_EDGE('',*,*,#3408,.T.);
#4508=ORIENTED_EDGE('',*,*,#3409,.T.);
#4509=ORIENTED_EDGE('',*,*,#3410,.F.);
#4510=ORIENTED_EDGE('',*,*,#3411,.F.);
#4511=ORIENTED_EDGE('',*,*,#3412,.T.);
#4512=ORIENTED_EDGE('',*,*,#3335,.T.);
#4513=ORIENTED_EDGE('',*,*,#3412,.F.);
#4514=ORIENTED_EDGE('',*,*,#3413,.F.);
#4515=ORIENTED_EDGE('',*,*,#3414,.T.);
#4516=ORIENTED_EDGE('',*,*,#3334,.T.);
#4517=ORIENTED_EDGE('',*,*,#3414,.F.);
#4518=ORIENTED_EDGE('',*,*,#3415,.F.);
#4519=ORIENTED_EDGE('',*,*,#3410,.T.);
#4520=ORIENTED_EDGE('',*,*,#3416,.F.);
#4521=ORIENTED_EDGE('',*,*,#3417,.F.);
#4522=ORIENTED_EDGE('',*,*,#3418,.F.);
#4523=ORIENTED_EDGE('',*,*,#3419,.F.);
#4524=ORIENTED_EDGE('',*,*,#3349,.T.);
#4525=ORIENTED_EDGE('',*,*,#3380,.F.);
#4526=ORIENTED_EDGE('',*,*,#3359,.T.);
#4527=ORIENTED_EDGE('',*,*,#3420,.T.);
#4528=ORIENTED_EDGE('',*,*,#3415,.T.);
#4529=ORIENTED_EDGE('',*,*,#3421,.T.);
#4530=ORIENTED_EDGE('',*,*,#3422,.T.);
#4531=ORIENTED_EDGE('',*,*,#3405,.F.);
#4532=ORIENTED_EDGE('',*,*,#3350,.T.);
#4533=ORIENTED_EDGE('',*,*,#3420,.F.);
#4534=ORIENTED_EDGE('',*,*,#3358,.T.);
#4535=ORIENTED_EDGE('',*,*,#3423,.F.);
#4536=ORIENTED_EDGE('',*,*,#3419,.T.);
#4537=ORIENTED_EDGE('',*,*,#3424,.F.);
#4538=ORIENTED_EDGE('',*,*,#3425,.F.);
#4539=ORIENTED_EDGE('',*,*,#3421,.F.);
#4540=ORIENTED_EDGE('',*,*,#3351,.T.);
#4541=ORIENTED_EDGE('',*,*,#3423,.T.);
#4542=ORIENTED_EDGE('',*,*,#3357,.T.);
#4543=ORIENTED_EDGE('',*,*,#3426,.T.);
#4544=ORIENTED_EDGE('',*,*,#3284,.T.);
#4545=ORIENTED_EDGE('',*,*,#3293,.T.);
#4546=ORIENTED_EDGE('',*,*,#3411,.T.);
#4547=ORIENTED_EDGE('',*,*,#3418,.T.);
#4548=ORIENTED_EDGE('',*,*,#3427,.T.);
#4549=ORIENTED_EDGE('',*,*,#3428,.T.);
#4550=ORIENTED_EDGE('',*,*,#3424,.T.);
#4551=ORIENTED_EDGE('',*,*,#3352,.T.);
#4552=ORIENTED_EDGE('',*,*,#3426,.F.);
#4553=ORIENTED_EDGE('',*,*,#3356,.T.);
#4554=ORIENTED_EDGE('',*,*,#3429,.F.);
#4555=ORIENTED_EDGE('',*,*,#3353,.T.);
#4556=ORIENTED_EDGE('',*,*,#3429,.T.);
#4557=ORIENTED_EDGE('',*,*,#3355,.T.);
#4558=ORIENTED_EDGE('',*,*,#3381,.F.);
#4559=ORIENTED_EDGE('',*,*,#3416,.T.);
#4560=ORIENTED_EDGE('',*,*,#3409,.F.);
#4561=ORIENTED_EDGE('',*,*,#3430,.T.);
#4562=ORIENTED_EDGE('',*,*,#3431,.T.);
#4563=ORIENTED_EDGE('',*,*,#3318,.T.);
#4564=ORIENTED_EDGE('',*,*,#3404,.T.);
#4565=ORIENTED_EDGE('',*,*,#3432,.F.);
#4566=ORIENTED_EDGE('',*,*,#3433,.F.);
#4567=ORIENTED_EDGE('',*,*,#3434,.F.);
#4568=ORIENTED_EDGE('',*,*,#3435,.F.);
#4569=ORIENTED_EDGE('',*,*,#3436,.F.);
#4570=ORIENTED_EDGE('',*,*,#3382,.T.);
#4571=ORIENTED_EDGE('',*,*,#3345,.T.);
#4572=ORIENTED_EDGE('',*,*,#3342,.T.);
#4573=ORIENTED_EDGE('',*,*,#3432,.T.);
#4574=ORIENTED_EDGE('',*,*,#3403,.F.);
#4575=ORIENTED_EDGE('',*,*,#3366,.T.);
#4576=ORIENTED_EDGE('',*,*,#3437,.T.);
#4577=ORIENTED_EDGE('',*,*,#3433,.T.);
#4578=ORIENTED_EDGE('',*,*,#3437,.F.);
#4579=ORIENTED_EDGE('',*,*,#3365,.T.);
#4580=ORIENTED_EDGE('',*,*,#3438,.F.);
#4581=ORIENTED_EDGE('',*,*,#3434,.T.);
#4582=ORIENTED_EDGE('',*,*,#3438,.T.);
#4583=ORIENTED_EDGE('',*,*,#3364,.T.);
#4584=ORIENTED_EDGE('',*,*,#3439,.T.);
#4585=ORIENTED_EDGE('',*,*,#3435,.T.);
#4586=ORIENTED_EDGE('',*,*,#3439,.F.);
#4587=ORIENTED_EDGE('',*,*,#3363,.T.);
#4588=ORIENTED_EDGE('',*,*,#3440,.F.);
#4589=ORIENTED_EDGE('',*,*,#3436,.T.);
#4590=ORIENTED_EDGE('',*,*,#3440,.T.);
#4591=ORIENTED_EDGE('',*,*,#3362,.T.);
#4592=ORIENTED_EDGE('',*,*,#3383,.F.);
#4593=ORIENTED_EDGE('',*,*,#3314,.T.);
#4594=ORIENTED_EDGE('',*,*,#3402,.T.);
#4595=ORIENTED_EDGE('',*,*,#3441,.F.);
#4596=ORIENTED_EDGE('',*,*,#3442,.F.);
#4597=ORIENTED_EDGE('',*,*,#3443,.F.);
#4598=ORIENTED_EDGE('',*,*,#3444,.F.);
#4599=ORIENTED_EDGE('',*,*,#3445,.F.);
#4600=ORIENTED_EDGE('',*,*,#3384,.T.);
#4601=ORIENTED_EDGE('',*,*,#3330,.T.);
#4602=ORIENTED_EDGE('',*,*,#3340,.T.);
#4603=ORIENTED_EDGE('',*,*,#3441,.T.);
#4604=ORIENTED_EDGE('',*,*,#3401,.F.);
#4605=ORIENTED_EDGE('',*,*,#3373,.T.);
#4606=ORIENTED_EDGE('',*,*,#3446,.T.);
#4607=ORIENTED_EDGE('',*,*,#3442,.T.);
#4608=ORIENTED_EDGE('',*,*,#3446,.F.);
#4609=ORIENTED_EDGE('',*,*,#3372,.T.);
#4610=ORIENTED_EDGE('',*,*,#3447,.F.);
#4611=ORIENTED_EDGE('',*,*,#3443,.T.);
#4612=ORIENTED_EDGE('',*,*,#3447,.T.);
#4613=ORIENTED_EDGE('',*,*,#3371,.T.);
#4614=ORIENTED_EDGE('',*,*,#3448,.T.);
#4615=ORIENTED_EDGE('',*,*,#3287,.T.);
#4616=ORIENTED_EDGE('',*,*,#3290,.T.);
#4617=ORIENTED_EDGE('',*,*,#3413,.T.);
#4618=ORIENTED_EDGE('',*,*,#3444,.T.);
#4619=ORIENTED_EDGE('',*,*,#3448,.F.);
#4620=ORIENTED_EDGE('',*,*,#3370,.T.);
#4621=ORIENTED_EDGE('',*,*,#3449,.F.);
#4622=ORIENTED_EDGE('',*,*,#3445,.T.);
#4623=ORIENTED_EDGE('',*,*,#3449,.T.);
#4624=ORIENTED_EDGE('',*,*,#3369,.T.);
#4625=ORIENTED_EDGE('',*,*,#3385,.F.);
#4626=ORIENTED_EDGE('',*,*,#3310,.T.);
#4627=ORIENTED_EDGE('',*,*,#3400,.T.);
#4628=ORIENTED_EDGE('',*,*,#3450,.F.);
#4629=ORIENTED_EDGE('',*,*,#3451,.F.);
#4630=ORIENTED_EDGE('',*,*,#3452,.F.);
#4631=ORIENTED_EDGE('',*,*,#3453,.F.);
#4632=ORIENTED_EDGE('',*,*,#3454,.F.);
#4633=ORIENTED_EDGE('',*,*,#3386,.T.);
#4634=ORIENTED_EDGE('',*,*,#3326,.T.);
#4635=ORIENTED_EDGE('',*,*,#3338,.T.);
#4636=ORIENTED_EDGE('',*,*,#3450,.T.);
#4637=ORIENTED_EDGE('',*,*,#3399,.F.);
#4638=ORIENTED_EDGE('',*,*,#3455,.T.);
#4639=ORIENTED_EDGE('',*,*,#3456,.T.);
#4640=ORIENTED_EDGE('',*,*,#3451,.T.);
#4641=ORIENTED_EDGE('',*,*,#3456,.F.);
#4642=ORIENTED_EDGE('',*,*,#3457,.F.);
#4643=ORIENTED_EDGE('',*,*,#3458,.F.);
#4644=ORIENTED_EDGE('',*,*,#3452,.T.);
#4645=ORIENTED_EDGE('',*,*,#3458,.T.);
#4646=ORIENTED_EDGE('',*,*,#3459,.T.);
#4647=ORIENTED_EDGE('',*,*,#3460,.T.);
#4648=ORIENTED_EDGE('',*,*,#3454,.T.);
#4649=ORIENTED_EDGE('',*,*,#3461,.T.);
#4650=ORIENTED_EDGE('',*,*,#3462,.T.);
#4651=ORIENTED_EDGE('',*,*,#3387,.F.);
#4652=ORIENTED_EDGE('',*,*,#3453,.T.);
#4653=ORIENTED_EDGE('',*,*,#3460,.F.);
#4654=ORIENTED_EDGE('',*,*,#3463,.F.);
#4655=ORIENTED_EDGE('',*,*,#3461,.F.);
#4656=ORIENTED_EDGE('',*,*,#3464,.T.);
#4657=ORIENTED_EDGE('',*,*,#3465,.T.);
#4658=ORIENTED_EDGE('',*,*,#3463,.T.);
#4659=ORIENTED_EDGE('',*,*,#3466,.T.);
#4660=ORIENTED_EDGE('',*,*,#3467,.T.);
#4661=ORIENTED_EDGE('',*,*,#3468,.T.);
#4662=ORIENTED_EDGE('',*,*,#3457,.T.);
#4663=ORIENTED_EDGE('',*,*,#3469,.T.);
#4664=ORIENTED_EDGE('',*,*,#3470,.T.);
#4665=ORIENTED_EDGE('',*,*,#3464,.F.);
#4666=ORIENTED_EDGE('',*,*,#3459,.F.);
#4667=ORIENTED_EDGE('',*,*,#3470,.F.);
#4668=ORIENTED_EDGE('',*,*,#3377,.F.);
#4669=ORIENTED_EDGE('',*,*,#3398,.F.);
#4670=ORIENTED_EDGE('',*,*,#3378,.F.);
#4671=ORIENTED_EDGE('',*,*,#3469,.F.);
#4672=ORIENTED_EDGE('',*,*,#3455,.F.);
#4673=ORIENTED_EDGE('',*,*,#3471,.T.);
#4674=ORIENTED_EDGE('',*,*,#3425,.T.);
#4675=ORIENTED_EDGE('',*,*,#3472,.T.);
#4676=ORIENTED_EDGE('',*,*,#3472,.F.);
#4677=ORIENTED_EDGE('',*,*,#3428,.F.);
#4678=ORIENTED_EDGE('',*,*,#3468,.F.);
#4679=ORIENTED_EDGE('',*,*,#3473,.F.);
#4680=ORIENTED_EDGE('',*,*,#3406,.F.);
#4681=ORIENTED_EDGE('',*,*,#3422,.F.);
#4682=ORIENTED_EDGE('',*,*,#3471,.F.);
#4683=ORIENTED_EDGE('',*,*,#3474,.F.);
#4684=ORIENTED_EDGE('',*,*,#3408,.F.);
#4685=ORIENTED_EDGE('',*,*,#3475,.F.);
#4686=ORIENTED_EDGE('',*,*,#3467,.F.);
#4687=ORIENTED_EDGE('',*,*,#3430,.F.);
#4688=ORIENTED_EDGE('',*,*,#3417,.T.);
#4689=ORIENTED_EDGE('',*,*,#3431,.F.);
#4690=ORIENTED_EDGE('',*,*,#3466,.F.);
#4691=ORIENTED_EDGE('',*,*,#3427,.F.);
#4692=ORIENTED_EDGE('',*,*,#3388,.F.);
#4693=ORIENTED_EDGE('',*,*,#3462,.F.);
#4694=ORIENTED_EDGE('',*,*,#3465,.F.);
#4695=ORIENTED_EDGE('',*,*,#3376,.F.);
#4696=ORIENTED_EDGE('',*,*,#3474,.T.);
#4697=ORIENTED_EDGE('',*,*,#3473,.T.);
#4698=ORIENTED_EDGE('',*,*,#3475,.T.);
#4699=ORIENTED_EDGE('',*,*,#3407,.F.);
#4700=ORIENTED_EDGE('',*,*,#3476,.F.);
#4701=ORIENTED_EDGE('',*,*,#3477,.F.);
#4702=ORIENTED_EDGE('',*,*,#3478,.F.);
#4703=ORIENTED_EDGE('',*,*,#3479,.F.);
#4704=ORIENTED_EDGE('',*,*,#3480,.F.);
#4705=ORIENTED_EDGE('',*,*,#3481,.F.);
#4706=ORIENTED_EDGE('',*,*,#3482,.F.);
#4707=ORIENTED_EDGE('',*,*,#3483,.F.);
#4708=ORIENTED_EDGE('',*,*,#3484,.F.);
#4709=ORIENTED_EDGE('',*,*,#3476,.T.);
#4710=ORIENTED_EDGE('',*,*,#3485,.T.);
#4711=ORIENTED_EDGE('',*,*,#3483,.T.);
#4712=ORIENTED_EDGE('',*,*,#3486,.T.);
#4713=ORIENTED_EDGE('',*,*,#3396,.T.);
#4714=ORIENTED_EDGE('',*,*,#3487,.T.);
#4715=ORIENTED_EDGE('',*,*,#3484,.T.);
#4716=ORIENTED_EDGE('',*,*,#3488,.T.);
#4717=ORIENTED_EDGE('',*,*,#3489,.F.);
#4718=ORIENTED_EDGE('',*,*,#3490,.F.);
#4719=ORIENTED_EDGE('',*,*,#3491,.F.);
#4720=ORIENTED_EDGE('',*,*,#3490,.T.);
#4721=ORIENTED_EDGE('',*,*,#3492,.T.);
#4722=ORIENTED_EDGE('',*,*,#3480,.T.);
#4723=ORIENTED_EDGE('',*,*,#3493,.T.);
#4724=ORIENTED_EDGE('',*,*,#3482,.T.);
#4725=ORIENTED_EDGE('',*,*,#3494,.T.);
#4726=ORIENTED_EDGE('',*,*,#3491,.T.);
#4727=ORIENTED_EDGE('',*,*,#3495,.T.);
#4728=ORIENTED_EDGE('',*,*,#3394,.T.);
#4729=ORIENTED_EDGE('',*,*,#3496,.T.);
#4730=ORIENTED_EDGE('',*,*,#3489,.T.);
#4731=ORIENTED_EDGE('',*,*,#3497,.T.);
#4732=ORIENTED_EDGE('',*,*,#3392,.T.);
#4733=ORIENTED_EDGE('',*,*,#3498,.T.);
#4734=ORIENTED_EDGE('',*,*,#3481,.T.);
#4735=ORIENTED_EDGE('',*,*,#3499,.T.);
#4736=ORIENTED_EDGE('',*,*,#3479,.T.);
#4737=ORIENTED_EDGE('',*,*,#3500,.T.);
#4738=ORIENTED_EDGE('',*,*,#3477,.T.);
#4739=ORIENTED_EDGE('',*,*,#3501,.T.);
#4740=ORIENTED_EDGE('',*,*,#3390,.T.);
#4741=ORIENTED_EDGE('',*,*,#3502,.T.);
#4742=ORIENTED_EDGE('',*,*,#3478,.T.);
#4743=ORIENTED_EDGE('',*,*,#3503,.T.);
#4744=ORIENTED_EDGE('',*,*,#3497,.F.);
#4745=ORIENTED_EDGE('',*,*,#3494,.F.);
#4746=ORIENTED_EDGE('',*,*,#3487,.F.);
#4747=ORIENTED_EDGE('',*,*,#3395,.F.);
#4748=ORIENTED_EDGE('',*,*,#3308,.T.);
#4749=ORIENTED_EDGE('',*,*,#3397,.F.);
#4750=ORIENTED_EDGE('',*,*,#3488,.F.);
#4751=ORIENTED_EDGE('',*,*,#3485,.F.);
#4752=ORIENTED_EDGE('',*,*,#3502,.F.);
#4753=ORIENTED_EDGE('',*,*,#3389,.F.);
#4754=ORIENTED_EDGE('',*,*,#3324,.T.);
#4755=ORIENTED_EDGE('',*,*,#3337,.T.);
#4756=ORIENTED_EDGE('',*,*,#3493,.F.);
#4757=ORIENTED_EDGE('',*,*,#3501,.F.);
#4758=ORIENTED_EDGE('',*,*,#3486,.F.);
#4759=ORIENTED_EDGE('',*,*,#3495,.F.);
#4760=ORIENTED_EDGE('',*,*,#3298,.T.);
#4761=ORIENTED_EDGE('',*,*,#3294,.T.);
#4762=ORIENTED_EDGE('',*,*,#3291,.T.);
#4763=ORIENTED_EDGE('',*,*,#3288,.T.);
#4764=ORIENTED_EDGE('',*,*,#3285,.T.);
#4765=ORIENTED_EDGE('',*,*,#3282,.T.);
#4766=ORIENTED_EDGE('',*,*,#3498,.F.);
#4767=ORIENTED_EDGE('',*,*,#3391,.F.);
#4768=ORIENTED_EDGE('',*,*,#3503,.F.);
#4769=ORIENTED_EDGE('',*,*,#3500,.F.);
#4770=ORIENTED_EDGE('',*,*,#3496,.F.);
#4771=ORIENTED_EDGE('',*,*,#3393,.F.);
#4772=ORIENTED_EDGE('',*,*,#3499,.F.);
#4773=ORIENTED_EDGE('',*,*,#3492,.F.);
#4774=ORIENTED_EDGE('',*,*,#3504,.F.);
#4775=ORIENTED_EDGE('',*,*,#3505,.T.);
#4776=ORIENTED_EDGE('',*,*,#3506,.F.);
#4777=ORIENTED_EDGE('',*,*,#3505,.F.);
#4778=ORIENTED_EDGE('',*,*,#3507,.F.);
#4779=ORIENTED_EDGE('',*,*,#3508,.T.);
#4780=ORIENTED_EDGE('',*,*,#3509,.F.);
#4781=ORIENTED_EDGE('',*,*,#3508,.F.);
#4782=ORIENTED_EDGE('',*,*,#3510,.F.);
#4783=ORIENTED_EDGE('',*,*,#3511,.T.);
#4784=ORIENTED_EDGE('',*,*,#3512,.F.);
#4785=ORIENTED_EDGE('',*,*,#3511,.F.);
#4786=ORIENTED_EDGE('',*,*,#3513,.F.);
#4787=ORIENTED_EDGE('',*,*,#3514,.T.);
#4788=ORIENTED_EDGE('',*,*,#3515,.F.);
#4789=ORIENTED_EDGE('',*,*,#3514,.F.);
#4790=ORIENTED_EDGE('',*,*,#3516,.F.);
#4791=ORIENTED_EDGE('',*,*,#3517,.T.);
#4792=ORIENTED_EDGE('',*,*,#3518,.T.);
#4793=ORIENTED_EDGE('',*,*,#3519,.F.);
#4794=ORIENTED_EDGE('',*,*,#3520,.F.);
#4795=ORIENTED_EDGE('',*,*,#3521,.T.);
#4796=ORIENTED_EDGE('',*,*,#3522,.T.);
#4797=ORIENTED_EDGE('',*,*,#3517,.F.);
#4798=ORIENTED_EDGE('',*,*,#3523,.F.);
#4799=ORIENTED_EDGE('',*,*,#3524,.T.);
#4800=ORIENTED_EDGE('',*,*,#3525,.T.);
#4801=ORIENTED_EDGE('',*,*,#3521,.F.);
#4802=ORIENTED_EDGE('',*,*,#3526,.F.);
#4803=ORIENTED_EDGE('',*,*,#3527,.T.);
#4804=ORIENTED_EDGE('',*,*,#3528,.T.);
#4805=ORIENTED_EDGE('',*,*,#3524,.F.);
#4806=ORIENTED_EDGE('',*,*,#3529,.F.);
#4807=ORIENTED_EDGE('',*,*,#3530,.T.);
#4808=ORIENTED_EDGE('',*,*,#3531,.T.);
#4809=ORIENTED_EDGE('',*,*,#3527,.F.);
#4810=ORIENTED_EDGE('',*,*,#3532,.F.);
#4811=ORIENTED_EDGE('',*,*,#3519,.T.);
#4812=ORIENTED_EDGE('',*,*,#3533,.T.);
#4813=ORIENTED_EDGE('',*,*,#3530,.F.);
#4814=ORIENTED_EDGE('',*,*,#3533,.F.);
#4815=ORIENTED_EDGE('',*,*,#3518,.F.);
#4816=ORIENTED_EDGE('',*,*,#3522,.F.);
#4817=ORIENTED_EDGE('',*,*,#3525,.F.);
#4818=ORIENTED_EDGE('',*,*,#3528,.F.);
#4819=ORIENTED_EDGE('',*,*,#3531,.F.);
#4820=ORIENTED_EDGE('',*,*,#3534,.F.);
#4821=ORIENTED_EDGE('',*,*,#3535,.F.);
#4822=ORIENTED_EDGE('',*,*,#3536,.T.);
#4823=ORIENTED_EDGE('',*,*,#3537,.T.);
#4824=ORIENTED_EDGE('',*,*,#3538,.F.);
#4825=ORIENTED_EDGE('',*,*,#3539,.F.);
#4826=ORIENTED_EDGE('',*,*,#3540,.T.);
#4827=ORIENTED_EDGE('',*,*,#3541,.T.);
#4828=ORIENTED_EDGE('',*,*,#3536,.F.);
#4829=ORIENTED_EDGE('',*,*,#3542,.F.);
#4830=ORIENTED_EDGE('',*,*,#3543,.T.);
#4831=ORIENTED_EDGE('',*,*,#3544,.T.);
#4832=ORIENTED_EDGE('',*,*,#3540,.F.);
#4833=ORIENTED_EDGE('',*,*,#3545,.F.);
#4834=ORIENTED_EDGE('',*,*,#3546,.T.);
#4835=ORIENTED_EDGE('',*,*,#3547,.T.);
#4836=ORIENTED_EDGE('',*,*,#3543,.F.);
#4837=ORIENTED_EDGE('',*,*,#3548,.F.);
#4838=ORIENTED_EDGE('',*,*,#3549,.T.);
#4839=ORIENTED_EDGE('',*,*,#3550,.T.);
#4840=ORIENTED_EDGE('',*,*,#3546,.F.);
#4841=ORIENTED_EDGE('',*,*,#3551,.F.);
#4842=ORIENTED_EDGE('',*,*,#3538,.T.);
#4843=ORIENTED_EDGE('',*,*,#3552,.T.);
#4844=ORIENTED_EDGE('',*,*,#3549,.F.);
#4845=ORIENTED_EDGE('',*,*,#3552,.F.);
#4846=ORIENTED_EDGE('',*,*,#3537,.F.);
#4847=ORIENTED_EDGE('',*,*,#3541,.F.);
#4848=ORIENTED_EDGE('',*,*,#3544,.F.);
#4849=ORIENTED_EDGE('',*,*,#3547,.F.);
#4850=ORIENTED_EDGE('',*,*,#3550,.F.);
#4851=ORIENTED_EDGE('',*,*,#3553,.F.);
#4852=ORIENTED_EDGE('',*,*,#3553,.T.);
#4853=ORIENTED_EDGE('',*,*,#3554,.T.);
#4854=ORIENTED_EDGE('',*,*,#3555,.F.);
#4855=ORIENTED_EDGE('',*,*,#3554,.F.);
#4856=ORIENTED_EDGE('',*,*,#3534,.T.);
#4857=ORIENTED_EDGE('',*,*,#3556,.T.);
#4858=ORIENTED_EDGE('',*,*,#3557,.F.);
#4859=ORIENTED_EDGE('',*,*,#3556,.F.);
#4860=ORIENTED_EDGE('',*,*,#3558,.F.);
#4861=ORIENTED_EDGE('',*,*,#3559,.F.);
#4862=ORIENTED_EDGE('',*,*,#3560,.F.);
#4863=ORIENTED_EDGE('',*,*,#3561,.T.);
#4864=ORIENTED_EDGE('',*,*,#3562,.F.);
#4865=ORIENTED_EDGE('',*,*,#3563,.T.);
#4866=ORIENTED_EDGE('',*,*,#3564,.F.);
#4867=ORIENTED_EDGE('',*,*,#3565,.F.);
#4868=ORIENTED_EDGE('',*,*,#3566,.F.);
#4869=ORIENTED_EDGE('',*,*,#3567,.T.);
#4870=ORIENTED_EDGE('',*,*,#3568,.F.);
#4871=ORIENTED_EDGE('',*,*,#3569,.F.);
#4872=ORIENTED_EDGE('',*,*,#3570,.F.);
#4873=ORIENTED_EDGE('',*,*,#3571,.T.);
#4874=ORIENTED_EDGE('',*,*,#3572,.F.);
#4875=ORIENTED_EDGE('',*,*,#3573,.F.);
#4876=ORIENTED_EDGE('',*,*,#3574,.F.);
#4877=ORIENTED_EDGE('',*,*,#3575,.T.);
#4878=ORIENTED_EDGE('',*,*,#3576,.F.);
#4879=ORIENTED_EDGE('',*,*,#3577,.F.);
#4880=ORIENTED_EDGE('',*,*,#3578,.F.);
#4881=ORIENTED_EDGE('',*,*,#3579,.F.);
#4882=ORIENTED_EDGE('',*,*,#3580,.F.);
#4883=ORIENTED_EDGE('',*,*,#3581,.T.);
#4884=ORIENTED_EDGE('',*,*,#3582,.F.);
#4885=ORIENTED_EDGE('',*,*,#3583,.F.);
#4886=ORIENTED_EDGE('',*,*,#3584,.F.);
#4887=ORIENTED_EDGE('',*,*,#3585,.T.);
#4888=ORIENTED_EDGE('',*,*,#3586,.F.);
#4889=ORIENTED_EDGE('',*,*,#3555,.T.);
#4890=ORIENTED_EDGE('',*,*,#3587,.F.);
#4891=ORIENTED_EDGE('',*,*,#3557,.T.);
#4892=ORIENTED_EDGE('',*,*,#3588,.F.);
#4893=ORIENTED_EDGE('',*,*,#3561,.F.);
#4894=ORIENTED_EDGE('',*,*,#3589,.F.);
#4895=ORIENTED_EDGE('',*,*,#3575,.F.);
#4896=ORIENTED_EDGE('',*,*,#3590,.F.);
#4897=ORIENTED_EDGE('',*,*,#3581,.F.);
#4898=ORIENTED_EDGE('',*,*,#3591,.F.);
#4899=ORIENTED_EDGE('',*,*,#3563,.F.);
#4900=ORIENTED_EDGE('',*,*,#3592,.F.);
#4901=ORIENTED_EDGE('',*,*,#3585,.F.);
#4902=ORIENTED_EDGE('',*,*,#3593,.F.);
#4903=ORIENTED_EDGE('',*,*,#3567,.F.);
#4904=ORIENTED_EDGE('',*,*,#3594,.F.);
#4905=ORIENTED_EDGE('',*,*,#3595,.F.);
#4906=ORIENTED_EDGE('',*,*,#3596,.F.);
#4907=ORIENTED_EDGE('',*,*,#3571,.F.);
#4908=ORIENTED_EDGE('',*,*,#3597,.F.);
#4909=ORIENTED_EDGE('',*,*,#3598,.F.);
#4910=ORIENTED_EDGE('',*,*,#3599,.F.);
#4911=ORIENTED_EDGE('',*,*,#3595,.T.);
#4912=ORIENTED_EDGE('',*,*,#3600,.T.);
#4913=ORIENTED_EDGE('',*,*,#3601,.F.);
#4914=ORIENTED_EDGE('',*,*,#3602,.F.);
#4915=ORIENTED_EDGE('',*,*,#3603,.F.);
#4916=ORIENTED_EDGE('',*,*,#3604,.F.);
#4917=ORIENTED_EDGE('',*,*,#3605,.F.);
#4918=ORIENTED_EDGE('',*,*,#3572,.T.);
#4919=ORIENTED_EDGE('',*,*,#3596,.T.);
#4920=ORIENTED_EDGE('',*,*,#3599,.T.);
#4921=ORIENTED_EDGE('',*,*,#3606,.T.);
#4922=ORIENTED_EDGE('',*,*,#3607,.F.);
#4923=ORIENTED_EDGE('',*,*,#3608,.F.);
#4924=ORIENTED_EDGE('',*,*,#3609,.F.);
#4925=ORIENTED_EDGE('',*,*,#3610,.F.);
#4926=ORIENTED_EDGE('',*,*,#3611,.F.);
#4927=ORIENTED_EDGE('',*,*,#3612,.T.);
#4928=ORIENTED_EDGE('',*,*,#3568,.T.);
#4929=ORIENTED_EDGE('',*,*,#3593,.T.);
#4930=ORIENTED_EDGE('',*,*,#3584,.T.);
#4931=ORIENTED_EDGE('',*,*,#3613,.T.);
#4932=ORIENTED_EDGE('',*,*,#3614,.F.);
#4933=ORIENTED_EDGE('',*,*,#3615,.F.);
#4934=ORIENTED_EDGE('',*,*,#3616,.F.);
#4935=ORIENTED_EDGE('',*,*,#3617,.F.);
#4936=ORIENTED_EDGE('',*,*,#3618,.F.);
#4937=ORIENTED_EDGE('',*,*,#3619,.T.);
#4938=ORIENTED_EDGE('',*,*,#3564,.T.);
#4939=ORIENTED_EDGE('',*,*,#3591,.T.);
#4940=ORIENTED_EDGE('',*,*,#3580,.T.);
#4941=ORIENTED_EDGE('',*,*,#3620,.T.);
#4942=ORIENTED_EDGE('',*,*,#3621,.F.);
#4943=ORIENTED_EDGE('',*,*,#3622,.F.);
#4944=ORIENTED_EDGE('',*,*,#3623,.F.);
#4945=ORIENTED_EDGE('',*,*,#3624,.F.);
#4946=ORIENTED_EDGE('',*,*,#3625,.F.);
#4947=ORIENTED_EDGE('',*,*,#3626,.T.);
#4948=ORIENTED_EDGE('',*,*,#3558,.T.);
#4949=ORIENTED_EDGE('',*,*,#3588,.T.);
#4950=ORIENTED_EDGE('',*,*,#3574,.T.);
#4951=ORIENTED_EDGE('',*,*,#3627,.F.);
#4952=ORIENTED_EDGE('',*,*,#3628,.T.);
#4953=ORIENTED_EDGE('',*,*,#3629,.T.);
#4954=ORIENTED_EDGE('',*,*,#3630,.T.);
#4955=ORIENTED_EDGE('',*,*,#3631,.F.);
#4956=ORIENTED_EDGE('',*,*,#3573,.T.);
#4957=ORIENTED_EDGE('',*,*,#3612,.F.);
#4958=ORIENTED_EDGE('',*,*,#3632,.T.);
#4959=ORIENTED_EDGE('',*,*,#3600,.F.);
#4960=ORIENTED_EDGE('',*,*,#3633,.T.);
#4961=ORIENTED_EDGE('',*,*,#3606,.F.);
#4962=ORIENTED_EDGE('',*,*,#3598,.T.);
#4963=ORIENTED_EDGE('',*,*,#3634,.F.);
#4964=ORIENTED_EDGE('',*,*,#3635,.T.);
#4965=ORIENTED_EDGE('',*,*,#3613,.F.);
#4966=ORIENTED_EDGE('',*,*,#3583,.T.);
#4967=ORIENTED_EDGE('',*,*,#3636,.F.);
#4968=ORIENTED_EDGE('',*,*,#3637,.T.);
#4969=ORIENTED_EDGE('',*,*,#3620,.F.);
#4970=ORIENTED_EDGE('',*,*,#3579,.T.);
#4971=ORIENTED_EDGE('',*,*,#3638,.F.);
#4972=ORIENTED_EDGE('',*,*,#3639,.T.);
#4973=ORIENTED_EDGE('',*,*,#3640,.T.);
#4974=ORIENTED_EDGE('',*,*,#3627,.T.);
#4975=ORIENTED_EDGE('',*,*,#3577,.T.);
#4976=ORIENTED_EDGE('',*,*,#3641,.T.);
#4977=ORIENTED_EDGE('',*,*,#3642,.F.);
#4978=ORIENTED_EDGE('',*,*,#3643,.T.);
#4979=ORIENTED_EDGE('',*,*,#3644,.F.);
#4980=ORIENTED_EDGE('',*,*,#3645,.T.);
#4981=ORIENTED_EDGE('',*,*,#3646,.F.);
#4982=ORIENTED_EDGE('',*,*,#3647,.T.);
#4983=ORIENTED_EDGE('',*,*,#3648,.F.);
#4984=ORIENTED_EDGE('',*,*,#3649,.T.);
#4985=ORIENTED_EDGE('',*,*,#3559,.T.);
#4986=ORIENTED_EDGE('',*,*,#3631,.T.);
#4987=ORIENTED_EDGE('',*,*,#3650,.T.);
#4988=ORIENTED_EDGE('',*,*,#3651,.T.);
#4989=ORIENTED_EDGE('',*,*,#3652,.F.);
#4990=ORIENTED_EDGE('',*,*,#3565,.T.);
#4991=ORIENTED_EDGE('',*,*,#3626,.F.);
#4992=ORIENTED_EDGE('',*,*,#3653,.T.);
#4993=ORIENTED_EDGE('',*,*,#3654,.F.);
#4994=ORIENTED_EDGE('',*,*,#3569,.T.);
#4995=ORIENTED_EDGE('',*,*,#3619,.F.);
#4996=ORIENTED_EDGE('',*,*,#3655,.T.);
#4997=ORIENTED_EDGE('',*,*,#3656,.F.);
#4998=ORIENTED_EDGE('',*,*,#3657,.T.);
#4999=ORIENTED_EDGE('',*,*,#3658,.T.);
#5000=ORIENTED_EDGE('',*,*,#3659,.T.);
#5001=ORIENTED_EDGE('',*,*,#3660,.T.);
#5002=ORIENTED_EDGE('',*,*,#3661,.T.);
#5003=ORIENTED_EDGE('',*,*,#3662,.F.);
#5004=ORIENTED_EDGE('',*,*,#3663,.F.);
#5005=ORIENTED_EDGE('',*,*,#3664,.T.);
#5006=ORIENTED_EDGE('',*,*,#3587,.T.);
#5007=ORIENTED_EDGE('',*,*,#3664,.F.);
#5008=ORIENTED_EDGE('',*,*,#3665,.F.);
#5009=ORIENTED_EDGE('',*,*,#3666,.T.);
#5010=ORIENTED_EDGE('',*,*,#3586,.T.);
#5011=ORIENTED_EDGE('',*,*,#3666,.F.);
#5012=ORIENTED_EDGE('',*,*,#3667,.F.);
#5013=ORIENTED_EDGE('',*,*,#3662,.T.);
#5014=ORIENTED_EDGE('',*,*,#3668,.F.);
#5015=ORIENTED_EDGE('',*,*,#3669,.F.);
#5016=ORIENTED_EDGE('',*,*,#3670,.F.);
#5017=ORIENTED_EDGE('',*,*,#3671,.F.);
#5018=ORIENTED_EDGE('',*,*,#3601,.T.);
#5019=ORIENTED_EDGE('',*,*,#3632,.F.);
#5020=ORIENTED_EDGE('',*,*,#3611,.T.);
#5021=ORIENTED_EDGE('',*,*,#3672,.T.);
#5022=ORIENTED_EDGE('',*,*,#3667,.T.);
#5023=ORIENTED_EDGE('',*,*,#3673,.T.);
#5024=ORIENTED_EDGE('',*,*,#3674,.T.);
#5025=ORIENTED_EDGE('',*,*,#3657,.F.);
#5026=ORIENTED_EDGE('',*,*,#3602,.T.);
#5027=ORIENTED_EDGE('',*,*,#3672,.F.);
#5028=ORIENTED_EDGE('',*,*,#3610,.T.);
#5029=ORIENTED_EDGE('',*,*,#3675,.F.);
#5030=ORIENTED_EDGE('',*,*,#3671,.T.);
#5031=ORIENTED_EDGE('',*,*,#3676,.F.);
#5032=ORIENTED_EDGE('',*,*,#3677,.F.);
#5033=ORIENTED_EDGE('',*,*,#3673,.F.);
#5034=ORIENTED_EDGE('',*,*,#3603,.T.);
#5035=ORIENTED_EDGE('',*,*,#3675,.T.);
#5036=ORIENTED_EDGE('',*,*,#3609,.T.);
#5037=ORIENTED_EDGE('',*,*,#3678,.T.);
#5038=ORIENTED_EDGE('',*,*,#3506,.T.);
#5039=ORIENTED_EDGE('',*,*,#3515,.T.);
#5040=ORIENTED_EDGE('',*,*,#3663,.T.);
#5041=ORIENTED_EDGE('',*,*,#3670,.T.);
#5042=ORIENTED_EDGE('',*,*,#3679,.T.);
#5043=ORIENTED_EDGE('',*,*,#3680,.T.);
#5044=ORIENTED_EDGE('',*,*,#3676,.T.);
#5045=ORIENTED_EDGE('',*,*,#3604,.T.);
#5046=ORIENTED_EDGE('',*,*,#3678,.F.);
#5047=ORIENTED_EDGE('',*,*,#3608,.T.);
#5048=ORIENTED_EDGE('',*,*,#3681,.F.);
#5049=ORIENTED_EDGE('',*,*,#3605,.T.);
#5050=ORIENTED_EDGE('',*,*,#3681,.T.);
#5051=ORIENTED_EDGE('',*,*,#3607,.T.);
#5052=ORIENTED_EDGE('',*,*,#3633,.F.);
#5053=ORIENTED_EDGE('',*,*,#3668,.T.);
#5054=ORIENTED_EDGE('',*,*,#3661,.F.);
#5055=ORIENTED_EDGE('',*,*,#3682,.T.);
#5056=ORIENTED_EDGE('',*,*,#3683,.T.);
#5057=ORIENTED_EDGE('',*,*,#3570,.T.);
#5058=ORIENTED_EDGE('',*,*,#3656,.T.);
#5059=ORIENTED_EDGE('',*,*,#3684,.F.);
#5060=ORIENTED_EDGE('',*,*,#3685,.F.);
#5061=ORIENTED_EDGE('',*,*,#3686,.F.);
#5062=ORIENTED_EDGE('',*,*,#3687,.F.);
#5063=ORIENTED_EDGE('',*,*,#3688,.F.);
#5064=ORIENTED_EDGE('',*,*,#3634,.T.);
#5065=ORIENTED_EDGE('',*,*,#3597,.T.);
#5066=ORIENTED_EDGE('',*,*,#3594,.T.);
#5067=ORIENTED_EDGE('',*,*,#3684,.T.);
#5068=ORIENTED_EDGE('',*,*,#3655,.F.);
#5069=ORIENTED_EDGE('',*,*,#3618,.T.);
#5070=ORIENTED_EDGE('',*,*,#3689,.T.);
#5071=ORIENTED_EDGE('',*,*,#3685,.T.);
#5072=ORIENTED_EDGE('',*,*,#3689,.F.);
#5073=ORIENTED_EDGE('',*,*,#3617,.T.);
#5074=ORIENTED_EDGE('',*,*,#3690,.F.);
#5075=ORIENTED_EDGE('',*,*,#3686,.T.);
#5076=ORIENTED_EDGE('',*,*,#3690,.T.);
#5077=ORIENTED_EDGE('',*,*,#3616,.T.);
#5078=ORIENTED_EDGE('',*,*,#3691,.T.);
#5079=ORIENTED_EDGE('',*,*,#3687,.T.);
#5080=ORIENTED_EDGE('',*,*,#3691,.F.);
#5081=ORIENTED_EDGE('',*,*,#3615,.T.);
#5082=ORIENTED_EDGE('',*,*,#3692,.F.);
#5083=ORIENTED_EDGE('',*,*,#3688,.T.);
#5084=ORIENTED_EDGE('',*,*,#3692,.T.);
#5085=ORIENTED_EDGE('',*,*,#3614,.T.);
#5086=ORIENTED_EDGE('',*,*,#3635,.F.);
#5087=ORIENTED_EDGE('',*,*,#3566,.T.);
#5088=ORIENTED_EDGE('',*,*,#3654,.T.);
#5089=ORIENTED_EDGE('',*,*,#3693,.F.);
#5090=ORIENTED_EDGE('',*,*,#3694,.F.);
#5091=ORIENTED_EDGE('',*,*,#3695,.F.);
#5092=ORIENTED_EDGE('',*,*,#3696,.F.);
#5093=ORIENTED_EDGE('',*,*,#3697,.F.);
#5094=ORIENTED_EDGE('',*,*,#3636,.T.);
#5095=ORIENTED_EDGE('',*,*,#3582,.T.);
#5096=ORIENTED_EDGE('',*,*,#3592,.T.);
#5097=ORIENTED_EDGE('',*,*,#3693,.T.);
#5098=ORIENTED_EDGE('',*,*,#3653,.F.);
#5099=ORIENTED_EDGE('',*,*,#3625,.T.);
#5100=ORIENTED_EDGE('',*,*,#3698,.T.);
#5101=ORIENTED_EDGE('',*,*,#3694,.T.);
#5102=ORIENTED_EDGE('',*,*,#3698,.F.);
#5103=ORIENTED_EDGE('',*,*,#3624,.T.);
#5104=ORIENTED_EDGE('',*,*,#3699,.F.);
#5105=ORIENTED_EDGE('',*,*,#3695,.T.);
#5106=ORIENTED_EDGE('',*,*,#3699,.T.);
#5107=ORIENTED_EDGE('',*,*,#3623,.T.);
#5108=ORIENTED_EDGE('',*,*,#3700,.T.);
#5109=ORIENTED_EDGE('',*,*,#3509,.T.);
#5110=ORIENTED_EDGE('',*,*,#3512,.T.);
#5111=ORIENTED_EDGE('',*,*,#3665,.T.);
#5112=ORIENTED_EDGE('',*,*,#3696,.T.);
#5113=ORIENTED_EDGE('',*,*,#3700,.F.);
#5114=ORIENTED_EDGE('',*,*,#3622,.T.);
#5115=ORIENTED_EDGE('',*,*,#3701,.F.);
#5116=ORIENTED_EDGE('',*,*,#3697,.T.);
#5117=ORIENTED_EDGE('',*,*,#3701,.T.);
#5118=ORIENTED_EDGE('',*,*,#3621,.T.);
#5119=ORIENTED_EDGE('',*,*,#3637,.F.);
#5120=ORIENTED_EDGE('',*,*,#3562,.T.);
#5121=ORIENTED_EDGE('',*,*,#3652,.T.);
#5122=ORIENTED_EDGE('',*,*,#3702,.F.);
#5123=ORIENTED_EDGE('',*,*,#3703,.F.);
#5124=ORIENTED_EDGE('',*,*,#3704,.F.);
#5125=ORIENTED_EDGE('',*,*,#3705,.F.);
#5126=ORIENTED_EDGE('',*,*,#3706,.F.);
#5127=ORIENTED_EDGE('',*,*,#3638,.T.);
#5128=ORIENTED_EDGE('',*,*,#3578,.T.);
#5129=ORIENTED_EDGE('',*,*,#3590,.T.);
#5130=ORIENTED_EDGE('',*,*,#3702,.T.);
#5131=ORIENTED_EDGE('',*,*,#3651,.F.);
#5132=ORIENTED_EDGE('',*,*,#3707,.T.);
#5133=ORIENTED_EDGE('',*,*,#3708,.T.);
#5134=ORIENTED_EDGE('',*,*,#3703,.T.);
#5135=ORIENTED_EDGE('',*,*,#3708,.F.);
#5136=ORIENTED_EDGE('',*,*,#3709,.F.);
#5137=ORIENTED_EDGE('',*,*,#3710,.F.);
#5138=ORIENTED_EDGE('',*,*,#3704,.T.);
#5139=ORIENTED_EDGE('',*,*,#3710,.T.);
#5140=ORIENTED_EDGE('',*,*,#3711,.T.);
#5141=ORIENTED_EDGE('',*,*,#3712,.T.);
#5142=ORIENTED_EDGE('',*,*,#3706,.T.);
#5143=ORIENTED_EDGE('',*,*,#3713,.T.);
#5144=ORIENTED_EDGE('',*,*,#3714,.T.);
#5145=ORIENTED_EDGE('',*,*,#3639,.F.);
#5146=ORIENTED_EDGE('',*,*,#3705,.T.);
#5147=ORIENTED_EDGE('',*,*,#3712,.F.);
#5148=ORIENTED_EDGE('',*,*,#3715,.F.);
#5149=ORIENTED_EDGE('',*,*,#3713,.F.);
#5150=ORIENTED_EDGE('',*,*,#3716,.T.);
#5151=ORIENTED_EDGE('',*,*,#3717,.T.);
#5152=ORIENTED_EDGE('',*,*,#3715,.T.);
#5153=ORIENTED_EDGE('',*,*,#3718,.T.);
#5154=ORIENTED_EDGE('',*,*,#3719,.T.);
#5155=ORIENTED_EDGE('',*,*,#3720,.T.);
#5156=ORIENTED_EDGE('',*,*,#3709,.T.);
#5157=ORIENTED_EDGE('',*,*,#3721,.T.);
#5158=ORIENTED_EDGE('',*,*,#3722,.T.);
#5159=ORIENTED_EDGE('',*,*,#3716,.F.);
#5160=ORIENTED_EDGE('',*,*,#3711,.F.);
#5161=ORIENTED_EDGE('',*,*,#3722,.F.);
#5162=ORIENTED_EDGE('',*,*,#3629,.F.);
#5163=ORIENTED_EDGE('',*,*,#3650,.F.);
#5164=ORIENTED_EDGE('',*,*,#3630,.F.);
#5165=ORIENTED_EDGE('',*,*,#3721,.F.);
#5166=ORIENTED_EDGE('',*,*,#3707,.F.);
#5167=ORIENTED_EDGE('',*,*,#3723,.T.);
#5168=ORIENTED_EDGE('',*,*,#3677,.T.);
#5169=ORIENTED_EDGE('',*,*,#3724,.T.);
#5170=ORIENTED_EDGE('',*,*,#3724,.F.);
#5171=ORIENTED_EDGE('',*,*,#3680,.F.);
#5172=ORIENTED_EDGE('',*,*,#3720,.F.);
#5173=ORIENTED_EDGE('',*,*,#3725,.F.);
#5174=ORIENTED_EDGE('',*,*,#3658,.F.);
#5175=ORIENTED_EDGE('',*,*,#3674,.F.);
#5176=ORIENTED_EDGE('',*,*,#3723,.F.);
#5177=ORIENTED_EDGE('',*,*,#3726,.F.);
#5178=ORIENTED_EDGE('',*,*,#3660,.F.);
#5179=ORIENTED_EDGE('',*,*,#3727,.F.);
#5180=ORIENTED_EDGE('',*,*,#3719,.F.);
#5181=ORIENTED_EDGE('',*,*,#3682,.F.);
#5182=ORIENTED_EDGE('',*,*,#3669,.T.);
#5183=ORIENTED_EDGE('',*,*,#3683,.F.);
#5184=ORIENTED_EDGE('',*,*,#3718,.F.);
#5185=ORIENTED_EDGE('',*,*,#3679,.F.);
#5186=ORIENTED_EDGE('',*,*,#3640,.F.);
#5187=ORIENTED_EDGE('',*,*,#3714,.F.);
#5188=ORIENTED_EDGE('',*,*,#3717,.F.);
#5189=ORIENTED_EDGE('',*,*,#3628,.F.);
#5190=ORIENTED_EDGE('',*,*,#3726,.T.);
#5191=ORIENTED_EDGE('',*,*,#3725,.T.);
#5192=ORIENTED_EDGE('',*,*,#3727,.T.);
#5193=ORIENTED_EDGE('',*,*,#3659,.F.);
#5194=ORIENTED_EDGE('',*,*,#3728,.F.);
#5195=ORIENTED_EDGE('',*,*,#3729,.F.);
#5196=ORIENTED_EDGE('',*,*,#3730,.F.);
#5197=ORIENTED_EDGE('',*,*,#3731,.F.);
#5198=ORIENTED_EDGE('',*,*,#3732,.F.);
#5199=ORIENTED_EDGE('',*,*,#3733,.F.);
#5200=ORIENTED_EDGE('',*,*,#3734,.F.);
#5201=ORIENTED_EDGE('',*,*,#3735,.F.);
#5202=ORIENTED_EDGE('',*,*,#3736,.F.);
#5203=ORIENTED_EDGE('',*,*,#3728,.T.);
#5204=ORIENTED_EDGE('',*,*,#3737,.T.);
#5205=ORIENTED_EDGE('',*,*,#3735,.T.);
#5206=ORIENTED_EDGE('',*,*,#3738,.T.);
#5207=ORIENTED_EDGE('',*,*,#3648,.T.);
#5208=ORIENTED_EDGE('',*,*,#3739,.T.);
#5209=ORIENTED_EDGE('',*,*,#3736,.T.);
#5210=ORIENTED_EDGE('',*,*,#3740,.T.);
#5211=ORIENTED_EDGE('',*,*,#3741,.F.);
#5212=ORIENTED_EDGE('',*,*,#3742,.F.);
#5213=ORIENTED_EDGE('',*,*,#3743,.F.);
#5214=ORIENTED_EDGE('',*,*,#3742,.T.);
#5215=ORIENTED_EDGE('',*,*,#3744,.T.);
#5216=ORIENTED_EDGE('',*,*,#3732,.T.);
#5217=ORIENTED_EDGE('',*,*,#3745,.T.);
#5218=ORIENTED_EDGE('',*,*,#3734,.T.);
#5219=ORIENTED_EDGE('',*,*,#3746,.T.);
#5220=ORIENTED_EDGE('',*,*,#3743,.T.);
#5221=ORIENTED_EDGE('',*,*,#3747,.T.);
#5222=ORIENTED_EDGE('',*,*,#3646,.T.);
#5223=ORIENTED_EDGE('',*,*,#3748,.T.);
#5224=ORIENTED_EDGE('',*,*,#3741,.T.);
#5225=ORIENTED_EDGE('',*,*,#3749,.T.);
#5226=ORIENTED_EDGE('',*,*,#3644,.T.);
#5227=ORIENTED_EDGE('',*,*,#3750,.T.);
#5228=ORIENTED_EDGE('',*,*,#3733,.T.);
#5229=ORIENTED_EDGE('',*,*,#3751,.T.);
#5230=ORIENTED_EDGE('',*,*,#3731,.T.);
#5231=ORIENTED_EDGE('',*,*,#3752,.T.);
#5232=ORIENTED_EDGE('',*,*,#3729,.T.);
#5233=ORIENTED_EDGE('',*,*,#3753,.T.);
#5234=ORIENTED_EDGE('',*,*,#3642,.T.);
#5235=ORIENTED_EDGE('',*,*,#3754,.T.);
#5236=ORIENTED_EDGE('',*,*,#3730,.T.);
#5237=ORIENTED_EDGE('',*,*,#3755,.T.);
#5238=ORIENTED_EDGE('',*,*,#3749,.F.);
#5239=ORIENTED_EDGE('',*,*,#3746,.F.);
#5240=ORIENTED_EDGE('',*,*,#3739,.F.);
#5241=ORIENTED_EDGE('',*,*,#3647,.F.);
#5242=ORIENTED_EDGE('',*,*,#3560,.T.);
#5243=ORIENTED_EDGE('',*,*,#3649,.F.);
#5244=ORIENTED_EDGE('',*,*,#3740,.F.);
#5245=ORIENTED_EDGE('',*,*,#3737,.F.);
#5246=ORIENTED_EDGE('',*,*,#3754,.F.);
#5247=ORIENTED_EDGE('',*,*,#3641,.F.);
#5248=ORIENTED_EDGE('',*,*,#3576,.T.);
#5249=ORIENTED_EDGE('',*,*,#3589,.T.);
#5250=ORIENTED_EDGE('',*,*,#3745,.F.);
#5251=ORIENTED_EDGE('',*,*,#3753,.F.);
#5252=ORIENTED_EDGE('',*,*,#3738,.F.);
#5253=ORIENTED_EDGE('',*,*,#3747,.F.);
#5254=ORIENTED_EDGE('',*,*,#3535,.T.);
#5255=ORIENTED_EDGE('',*,*,#3551,.T.);
#5256=ORIENTED_EDGE('',*,*,#3548,.T.);
#5257=ORIENTED_EDGE('',*,*,#3545,.T.);
#5258=ORIENTED_EDGE('',*,*,#3542,.T.);
#5259=ORIENTED_EDGE('',*,*,#3539,.T.);
#5260=ORIENTED_EDGE('',*,*,#3516,.T.);
#5261=ORIENTED_EDGE('',*,*,#3532,.T.);
#5262=ORIENTED_EDGE('',*,*,#3529,.T.);
#5263=ORIENTED_EDGE('',*,*,#3526,.T.);
#5264=ORIENTED_EDGE('',*,*,#3523,.T.);
#5265=ORIENTED_EDGE('',*,*,#3520,.T.);
#5266=ORIENTED_EDGE('',*,*,#3513,.T.);
#5267=ORIENTED_EDGE('',*,*,#3510,.T.);
#5268=ORIENTED_EDGE('',*,*,#3507,.T.);
#5269=ORIENTED_EDGE('',*,*,#3504,.T.);
#5270=ORIENTED_EDGE('',*,*,#3750,.F.);
#5271=ORIENTED_EDGE('',*,*,#3643,.F.);
#5272=ORIENTED_EDGE('',*,*,#3755,.F.);
#5273=ORIENTED_EDGE('',*,*,#3752,.F.);
#5274=ORIENTED_EDGE('',*,*,#3748,.F.);
#5275=ORIENTED_EDGE('',*,*,#3645,.F.);
#5276=ORIENTED_EDGE('',*,*,#3751,.F.);
#5277=ORIENTED_EDGE('',*,*,#3744,.F.);
#5278=ORIENTED_EDGE('',*,*,#3756,.F.);
#5279=ORIENTED_EDGE('',*,*,#3757,.T.);
#5280=ORIENTED_EDGE('',*,*,#3758,.F.);
#5281=ORIENTED_EDGE('',*,*,#3757,.F.);
#5282=ORIENTED_EDGE('',*,*,#3759,.F.);
#5283=ORIENTED_EDGE('',*,*,#3760,.T.);
#5284=ORIENTED_EDGE('',*,*,#3761,.F.);
#5285=ORIENTED_EDGE('',*,*,#3760,.F.);
#5286=ORIENTED_EDGE('',*,*,#3762,.T.);
#5287=ORIENTED_EDGE('',*,*,#3763,.T.);
#5288=ORIENTED_EDGE('',*,*,#3764,.F.);
#5289=ORIENTED_EDGE('',*,*,#3765,.T.);
#5290=ORIENTED_EDGE('',*,*,#3762,.F.);
#5291=ORIENTED_EDGE('',*,*,#3765,.F.);
#5292=ORIENTED_EDGE('',*,*,#3764,.T.);
#5293=ORIENTED_EDGE('',*,*,#3766,.T.);
#5294=ORIENTED_EDGE('',*,*,#3767,.T.);
#5295=ORIENTED_EDGE('',*,*,#3768,.F.);
#5296=ORIENTED_EDGE('',*,*,#3769,.T.);
#5297=ORIENTED_EDGE('',*,*,#3766,.F.);
#5298=ORIENTED_EDGE('',*,*,#3769,.F.);
#5299=ORIENTED_EDGE('',*,*,#3768,.T.);
#5300=ORIENTED_EDGE('',*,*,#3770,.T.);
#5301=ORIENTED_EDGE('',*,*,#3771,.T.);
#5302=ORIENTED_EDGE('',*,*,#3772,.F.);
#5303=ORIENTED_EDGE('',*,*,#3773,.T.);
#5304=ORIENTED_EDGE('',*,*,#3770,.F.);
#5305=ORIENTED_EDGE('',*,*,#3773,.F.);
#5306=ORIENTED_EDGE('',*,*,#3772,.T.);
#5307=ORIENTED_EDGE('',*,*,#3774,.T.);
#5308=ORIENTED_EDGE('',*,*,#3775,.T.);
#5309=ORIENTED_EDGE('',*,*,#3776,.F.);
#5310=ORIENTED_EDGE('',*,*,#3777,.T.);
#5311=ORIENTED_EDGE('',*,*,#3774,.F.);
#5312=ORIENTED_EDGE('',*,*,#3777,.F.);
#5313=ORIENTED_EDGE('',*,*,#3776,.T.);
#5314=ORIENTED_EDGE('',*,*,#3763,.F.);
#5315=ORIENTED_EDGE('',*,*,#3778,.T.);
#5316=ORIENTED_EDGE('',*,*,#3779,.F.);
#5317=ORIENTED_EDGE('',*,*,#3778,.F.);
#5318=ORIENTED_EDGE('',*,*,#3767,.F.);
#5319=ORIENTED_EDGE('',*,*,#3780,.T.);
#5320=ORIENTED_EDGE('',*,*,#3781,.F.);
#5321=ORIENTED_EDGE('',*,*,#3780,.F.);
#5322=ORIENTED_EDGE('',*,*,#3771,.F.);
#5323=ORIENTED_EDGE('',*,*,#3782,.T.);
#5324=ORIENTED_EDGE('',*,*,#3783,.F.);
#5325=ORIENTED_EDGE('',*,*,#3782,.F.);
#5326=ORIENTED_EDGE('',*,*,#3775,.F.);
#5327=ORIENTED_EDGE('',*,*,#3784,.T.);
#5328=ORIENTED_EDGE('',*,*,#3785,.F.);
#5329=ORIENTED_EDGE('',*,*,#3784,.F.);
#5330=ORIENTED_EDGE('',*,*,#3786,.T.);
#5331=ORIENTED_EDGE('',*,*,#3787,.T.);
#5332=ORIENTED_EDGE('',*,*,#3788,.T.);
#5333=ORIENTED_EDGE('',*,*,#3789,.T.);
#5334=ORIENTED_EDGE('',*,*,#3790,.T.);
#5335=ORIENTED_EDGE('',*,*,#3791,.T.);
#5336=ORIENTED_EDGE('',*,*,#3786,.F.);
#5337=ORIENTED_EDGE('',*,*,#3792,.T.);
#5338=ORIENTED_EDGE('',*,*,#3793,.T.);
#5339=ORIENTED_EDGE('',*,*,#3794,.T.);
#5340=ORIENTED_EDGE('',*,*,#3790,.F.);
#5341=ORIENTED_EDGE('',*,*,#3795,.T.);
#5342=ORIENTED_EDGE('',*,*,#3796,.T.);
#5343=ORIENTED_EDGE('',*,*,#3797,.T.);
#5344=ORIENTED_EDGE('',*,*,#3793,.F.);
#5345=ORIENTED_EDGE('',*,*,#3798,.T.);
#5346=ORIENTED_EDGE('',*,*,#3799,.T.);
#5347=ORIENTED_EDGE('',*,*,#3800,.T.);
#5348=ORIENTED_EDGE('',*,*,#3796,.F.);
#5349=ORIENTED_EDGE('',*,*,#3801,.T.);
#5350=ORIENTED_EDGE('',*,*,#3802,.T.);
#5351=ORIENTED_EDGE('',*,*,#3803,.T.);
#5352=ORIENTED_EDGE('',*,*,#3799,.F.);
#5353=ORIENTED_EDGE('',*,*,#3804,.T.);
#5354=ORIENTED_EDGE('',*,*,#3805,.T.);
#5355=ORIENTED_EDGE('',*,*,#3806,.T.);
#5356=ORIENTED_EDGE('',*,*,#3802,.F.);
#5357=ORIENTED_EDGE('',*,*,#3807,.T.);
#5358=ORIENTED_EDGE('',*,*,#3788,.F.);
#5359=ORIENTED_EDGE('',*,*,#3808,.T.);
#5360=ORIENTED_EDGE('',*,*,#3805,.F.);
#5361=ORIENTED_EDGE('',*,*,#3809,.T.);
#5362=ORIENTED_EDGE('',*,*,#3803,.F.);
#5363=ORIENTED_EDGE('',*,*,#3810,.F.);
#5364=ORIENTED_EDGE('',*,*,#3811,.F.);
#5365=ORIENTED_EDGE('',*,*,#3812,.F.);
#5366=ORIENTED_EDGE('',*,*,#3806,.F.);
#5367=ORIENTED_EDGE('',*,*,#3813,.T.);
#5368=ORIENTED_EDGE('',*,*,#3814,.T.);
#5369=ORIENTED_EDGE('',*,*,#3810,.T.);
#5370=ORIENTED_EDGE('',*,*,#3808,.F.);
#5371=ORIENTED_EDGE('',*,*,#3815,.F.);
#5372=ORIENTED_EDGE('',*,*,#3816,.F.);
#5373=ORIENTED_EDGE('',*,*,#3813,.F.);
#5374=ORIENTED_EDGE('',*,*,#3787,.F.);
#5375=ORIENTED_EDGE('',*,*,#3817,.T.);
#5376=ORIENTED_EDGE('',*,*,#3818,.T.);
#5377=ORIENTED_EDGE('',*,*,#3815,.T.);
#5378=ORIENTED_EDGE('',*,*,#3789,.F.);
#5379=ORIENTED_EDGE('',*,*,#3809,.F.);
#5380=ORIENTED_EDGE('',*,*,#3807,.F.);
#5381=ORIENTED_EDGE('',*,*,#3804,.F.);
#5382=ORIENTED_EDGE('',*,*,#3801,.F.);
#5383=ORIENTED_EDGE('',*,*,#3798,.F.);
#5384=ORIENTED_EDGE('',*,*,#3795,.F.);
#5385=ORIENTED_EDGE('',*,*,#3792,.F.);
#5386=ORIENTED_EDGE('',*,*,#3756,.T.);
#5387=ORIENTED_EDGE('',*,*,#3759,.T.);
#5388=ORIENTED_EDGE('',*,*,#3791,.F.);
#5389=ORIENTED_EDGE('',*,*,#3819,.F.);
#5390=ORIENTED_EDGE('',*,*,#3820,.F.);
#5391=ORIENTED_EDGE('',*,*,#3817,.F.);
#5392=ORIENTED_EDGE('',*,*,#3800,.F.);
#5393=ORIENTED_EDGE('',*,*,#3812,.T.);
#5394=ORIENTED_EDGE('',*,*,#3821,.T.);
#5395=ORIENTED_EDGE('',*,*,#3822,.T.);
#5396=ORIENTED_EDGE('',*,*,#3794,.F.);
#5397=ORIENTED_EDGE('',*,*,#3823,.T.);
#5398=ORIENTED_EDGE('',*,*,#3824,.T.);
#5399=ORIENTED_EDGE('',*,*,#3819,.T.);
#5400=ORIENTED_EDGE('',*,*,#3818,.F.);
#5401=ORIENTED_EDGE('',*,*,#3820,.T.);
#5402=ORIENTED_EDGE('',*,*,#3824,.F.);
#5403=ORIENTED_EDGE('',*,*,#3825,.T.);
#5404=ORIENTED_EDGE('',*,*,#3821,.F.);
#5405=ORIENTED_EDGE('',*,*,#3811,.T.);
#5406=ORIENTED_EDGE('',*,*,#3814,.F.);
#5407=ORIENTED_EDGE('',*,*,#3816,.T.);
#5408=ORIENTED_EDGE('',*,*,#3758,.T.);
#5409=ORIENTED_EDGE('',*,*,#3761,.T.);
#5410=ORIENTED_EDGE('',*,*,#3779,.T.);
#5411=ORIENTED_EDGE('',*,*,#3781,.T.);
#5412=ORIENTED_EDGE('',*,*,#3783,.T.);
#5413=ORIENTED_EDGE('',*,*,#3785,.T.);
#5414=ORIENTED_EDGE('',*,*,#3797,.F.);
#5415=ORIENTED_EDGE('',*,*,#3822,.F.);
#5416=ORIENTED_EDGE('',*,*,#3825,.F.);
#5417=ORIENTED_EDGE('',*,*,#3823,.F.);
#5418=ORIENTED_EDGE('',*,*,#3826,.F.);
#5419=ORIENTED_EDGE('',*,*,#3827,.T.);
#5420=ORIENTED_EDGE('',*,*,#3828,.T.);
#5421=ORIENTED_EDGE('',*,*,#3829,.T.);
#5422=ORIENTED_EDGE('',*,*,#3830,.F.);
#5423=ORIENTED_EDGE('',*,*,#3831,.T.);
#5424=ORIENTED_EDGE('',*,*,#3826,.T.);
#5425=ORIENTED_EDGE('',*,*,#3832,.T.);
#5426=ORIENTED_EDGE('',*,*,#3833,.F.);
#5427=ORIENTED_EDGE('',*,*,#3834,.T.);
#5428=ORIENTED_EDGE('',*,*,#3830,.T.);
#5429=ORIENTED_EDGE('',*,*,#3835,.T.);
#5430=ORIENTED_EDGE('',*,*,#3836,.F.);
#5431=ORIENTED_EDGE('',*,*,#3837,.T.);
#5432=ORIENTED_EDGE('',*,*,#3833,.T.);
#5433=ORIENTED_EDGE('',*,*,#3838,.T.);
#5434=ORIENTED_EDGE('',*,*,#3839,.F.);
#5435=ORIENTED_EDGE('',*,*,#3840,.T.);
#5436=ORIENTED_EDGE('',*,*,#3836,.T.);
#5437=ORIENTED_EDGE('',*,*,#3841,.T.);
#5438=ORIENTED_EDGE('',*,*,#3842,.F.);
#5439=ORIENTED_EDGE('',*,*,#3843,.T.);
#5440=ORIENTED_EDGE('',*,*,#3839,.T.);
#5441=ORIENTED_EDGE('',*,*,#3844,.T.);
#5442=ORIENTED_EDGE('',*,*,#3845,.F.);
#5443=ORIENTED_EDGE('',*,*,#3846,.T.);
#5444=ORIENTED_EDGE('',*,*,#3842,.T.);
#5445=ORIENTED_EDGE('',*,*,#3847,.T.);
#5446=ORIENTED_EDGE('',*,*,#3848,.F.);
#5447=ORIENTED_EDGE('',*,*,#3849,.T.);
#5448=ORIENTED_EDGE('',*,*,#3845,.T.);
#5449=ORIENTED_EDGE('',*,*,#3850,.T.);
#5450=ORIENTED_EDGE('',*,*,#3851,.F.);
#5451=ORIENTED_EDGE('',*,*,#3852,.T.);
#5452=ORIENTED_EDGE('',*,*,#3848,.T.);
#5453=ORIENTED_EDGE('',*,*,#3853,.T.);
#5454=ORIENTED_EDGE('',*,*,#3854,.F.);
#5455=ORIENTED_EDGE('',*,*,#3855,.T.);
#5456=ORIENTED_EDGE('',*,*,#3851,.T.);
#5457=ORIENTED_EDGE('',*,*,#3856,.T.);
#5458=ORIENTED_EDGE('',*,*,#3857,.F.);
#5459=ORIENTED_EDGE('',*,*,#3858,.T.);
#5460=ORIENTED_EDGE('',*,*,#3854,.T.);
#5461=ORIENTED_EDGE('',*,*,#3859,.T.);
#5462=ORIENTED_EDGE('',*,*,#3860,.F.);
#5463=ORIENTED_EDGE('',*,*,#3861,.T.);
#5464=ORIENTED_EDGE('',*,*,#3857,.T.);
#5465=ORIENTED_EDGE('',*,*,#3862,.T.);
#5466=ORIENTED_EDGE('',*,*,#3863,.F.);
#5467=ORIENTED_EDGE('',*,*,#3864,.T.);
#5468=ORIENTED_EDGE('',*,*,#3860,.T.);
#5469=ORIENTED_EDGE('',*,*,#3865,.T.);
#5470=ORIENTED_EDGE('',*,*,#3866,.F.);
#5471=ORIENTED_EDGE('',*,*,#3867,.T.);
#5472=ORIENTED_EDGE('',*,*,#3863,.T.);
#5473=ORIENTED_EDGE('',*,*,#3868,.T.);
#5474=ORIENTED_EDGE('',*,*,#3869,.F.);
#5475=ORIENTED_EDGE('',*,*,#3870,.T.);
#5476=ORIENTED_EDGE('',*,*,#3866,.T.);
#5477=ORIENTED_EDGE('',*,*,#3871,.T.);
#5478=ORIENTED_EDGE('',*,*,#3872,.F.);
#5479=ORIENTED_EDGE('',*,*,#3873,.T.);
#5480=ORIENTED_EDGE('',*,*,#3869,.T.);
#5481=ORIENTED_EDGE('',*,*,#3874,.T.);
#5482=ORIENTED_EDGE('',*,*,#3875,.F.);
#5483=ORIENTED_EDGE('',*,*,#3876,.T.);
#5484=ORIENTED_EDGE('',*,*,#3872,.T.);
#5485=ORIENTED_EDGE('',*,*,#3877,.T.);
#5486=ORIENTED_EDGE('',*,*,#3878,.F.);
#5487=ORIENTED_EDGE('',*,*,#3879,.T.);
#5488=ORIENTED_EDGE('',*,*,#3875,.T.);
#5489=ORIENTED_EDGE('',*,*,#3880,.T.);
#5490=ORIENTED_EDGE('',*,*,#3881,.F.);
#5491=ORIENTED_EDGE('',*,*,#3882,.T.);
#5492=ORIENTED_EDGE('',*,*,#3878,.T.);
#5493=ORIENTED_EDGE('',*,*,#3883,.T.);
#5494=ORIENTED_EDGE('',*,*,#3884,.F.);
#5495=ORIENTED_EDGE('',*,*,#3885,.T.);
#5496=ORIENTED_EDGE('',*,*,#3881,.T.);
#5497=ORIENTED_EDGE('',*,*,#3886,.T.);
#5498=ORIENTED_EDGE('',*,*,#3887,.F.);
#5499=ORIENTED_EDGE('',*,*,#3888,.T.);
#5500=ORIENTED_EDGE('',*,*,#3884,.T.);
#5501=ORIENTED_EDGE('',*,*,#3889,.T.);
#5502=ORIENTED_EDGE('',*,*,#3890,.F.);
#5503=ORIENTED_EDGE('',*,*,#3891,.T.);
#5504=ORIENTED_EDGE('',*,*,#3887,.T.);
#5505=ORIENTED_EDGE('',*,*,#3892,.T.);
#5506=ORIENTED_EDGE('',*,*,#3893,.F.);
#5507=ORIENTED_EDGE('',*,*,#3894,.T.);
#5508=ORIENTED_EDGE('',*,*,#3890,.T.);
#5509=ORIENTED_EDGE('',*,*,#3895,.T.);
#5510=ORIENTED_EDGE('',*,*,#3896,.F.);
#5511=ORIENTED_EDGE('',*,*,#3897,.T.);
#5512=ORIENTED_EDGE('',*,*,#3893,.T.);
#5513=ORIENTED_EDGE('',*,*,#3898,.T.);
#5514=ORIENTED_EDGE('',*,*,#3899,.F.);
#5515=ORIENTED_EDGE('',*,*,#3900,.T.);
#5516=ORIENTED_EDGE('',*,*,#3896,.T.);
#5517=ORIENTED_EDGE('',*,*,#3901,.T.);
#5518=ORIENTED_EDGE('',*,*,#3902,.F.);
#5519=ORIENTED_EDGE('',*,*,#3903,.T.);
#5520=ORIENTED_EDGE('',*,*,#3899,.T.);
#5521=ORIENTED_EDGE('',*,*,#3904,.T.);
#5522=ORIENTED_EDGE('',*,*,#3905,.F.);
#5523=ORIENTED_EDGE('',*,*,#3906,.T.);
#5524=ORIENTED_EDGE('',*,*,#3902,.T.);
#5525=ORIENTED_EDGE('',*,*,#3907,.T.);
#5526=ORIENTED_EDGE('',*,*,#3908,.F.);
#5527=ORIENTED_EDGE('',*,*,#3909,.T.);
#5528=ORIENTED_EDGE('',*,*,#3905,.T.);
#5529=ORIENTED_EDGE('',*,*,#3910,.T.);
#5530=ORIENTED_EDGE('',*,*,#3911,.F.);
#5531=ORIENTED_EDGE('',*,*,#3912,.T.);
#5532=ORIENTED_EDGE('',*,*,#3908,.T.);
#5533=ORIENTED_EDGE('',*,*,#3913,.T.);
#5534=ORIENTED_EDGE('',*,*,#3914,.F.);
#5535=ORIENTED_EDGE('',*,*,#3915,.T.);
#5536=ORIENTED_EDGE('',*,*,#3911,.T.);
#5537=ORIENTED_EDGE('',*,*,#3916,.T.);
#5538=ORIENTED_EDGE('',*,*,#3917,.F.);
#5539=ORIENTED_EDGE('',*,*,#3918,.T.);
#5540=ORIENTED_EDGE('',*,*,#3919,.T.);
#5541=ORIENTED_EDGE('',*,*,#3920,.F.);
#5542=ORIENTED_EDGE('',*,*,#3921,.F.);
#5543=ORIENTED_EDGE('',*,*,#3922,.T.);
#5544=ORIENTED_EDGE('',*,*,#3917,.T.);
#5545=ORIENTED_EDGE('',*,*,#3923,.F.);
#5546=ORIENTED_EDGE('',*,*,#3924,.F.);
#5547=ORIENTED_EDGE('',*,*,#3925,.T.);
#5548=ORIENTED_EDGE('',*,*,#3921,.T.);
#5549=ORIENTED_EDGE('',*,*,#3926,.F.);
#5550=ORIENTED_EDGE('',*,*,#3927,.F.);
#5551=ORIENTED_EDGE('',*,*,#3928,.T.);
#5552=ORIENTED_EDGE('',*,*,#3924,.T.);
#5553=ORIENTED_EDGE('',*,*,#3929,.F.);
#5554=ORIENTED_EDGE('',*,*,#3930,.F.);
#5555=ORIENTED_EDGE('',*,*,#3931,.T.);
#5556=ORIENTED_EDGE('',*,*,#3927,.T.);
#5557=ORIENTED_EDGE('',*,*,#3932,.F.);
#5558=ORIENTED_EDGE('',*,*,#3933,.F.);
#5559=ORIENTED_EDGE('',*,*,#3934,.T.);
#5560=ORIENTED_EDGE('',*,*,#3930,.T.);
#5561=ORIENTED_EDGE('',*,*,#3935,.F.);
#5562=ORIENTED_EDGE('',*,*,#3936,.F.);
#5563=ORIENTED_EDGE('',*,*,#3937,.T.);
#5564=ORIENTED_EDGE('',*,*,#3933,.T.);
#5565=ORIENTED_EDGE('',*,*,#3938,.F.);
#5566=ORIENTED_EDGE('',*,*,#3939,.F.);
#5567=ORIENTED_EDGE('',*,*,#3940,.T.);
#5568=ORIENTED_EDGE('',*,*,#3936,.T.);
#5569=ORIENTED_EDGE('',*,*,#3941,.F.);
#5570=ORIENTED_EDGE('',*,*,#3942,.F.);
#5571=ORIENTED_EDGE('',*,*,#3943,.T.);
#5572=ORIENTED_EDGE('',*,*,#3939,.T.);
#5573=ORIENTED_EDGE('',*,*,#3944,.F.);
#5574=ORIENTED_EDGE('',*,*,#3945,.F.);
#5575=ORIENTED_EDGE('',*,*,#3946,.T.);
#5576=ORIENTED_EDGE('',*,*,#3942,.T.);
#5577=ORIENTED_EDGE('',*,*,#3947,.F.);
#5578=ORIENTED_EDGE('',*,*,#3948,.F.);
#5579=ORIENTED_EDGE('',*,*,#3949,.T.);
#5580=ORIENTED_EDGE('',*,*,#3945,.T.);
#5581=ORIENTED_EDGE('',*,*,#3950,.F.);
#5582=ORIENTED_EDGE('',*,*,#3951,.F.);
#5583=ORIENTED_EDGE('',*,*,#3952,.T.);
#5584=ORIENTED_EDGE('',*,*,#3948,.T.);
#5585=ORIENTED_EDGE('',*,*,#3953,.F.);
#5586=ORIENTED_EDGE('',*,*,#3954,.F.);
#5587=ORIENTED_EDGE('',*,*,#3955,.T.);
#5588=ORIENTED_EDGE('',*,*,#3951,.T.);
#5589=ORIENTED_EDGE('',*,*,#3956,.F.);
#5590=ORIENTED_EDGE('',*,*,#3957,.F.);
#5591=ORIENTED_EDGE('',*,*,#3958,.T.);
#5592=ORIENTED_EDGE('',*,*,#3954,.T.);
#5593=ORIENTED_EDGE('',*,*,#3959,.F.);
#5594=ORIENTED_EDGE('',*,*,#3960,.F.);
#5595=ORIENTED_EDGE('',*,*,#3961,.T.);
#5596=ORIENTED_EDGE('',*,*,#3957,.T.);
#5597=ORIENTED_EDGE('',*,*,#3962,.F.);
#5598=ORIENTED_EDGE('',*,*,#3963,.F.);
#5599=ORIENTED_EDGE('',*,*,#3964,.T.);
#5600=ORIENTED_EDGE('',*,*,#3960,.T.);
#5601=ORIENTED_EDGE('',*,*,#3965,.F.);
#5602=ORIENTED_EDGE('',*,*,#3966,.F.);
#5603=ORIENTED_EDGE('',*,*,#3967,.T.);
#5604=ORIENTED_EDGE('',*,*,#3963,.T.);
#5605=ORIENTED_EDGE('',*,*,#3968,.F.);
#5606=ORIENTED_EDGE('',*,*,#3969,.F.);
#5607=ORIENTED_EDGE('',*,*,#3970,.T.);
#5608=ORIENTED_EDGE('',*,*,#3966,.T.);
#5609=ORIENTED_EDGE('',*,*,#3971,.F.);
#5610=ORIENTED_EDGE('',*,*,#3972,.F.);
#5611=ORIENTED_EDGE('',*,*,#3973,.T.);
#5612=ORIENTED_EDGE('',*,*,#3969,.T.);
#5613=ORIENTED_EDGE('',*,*,#3974,.F.);
#5614=ORIENTED_EDGE('',*,*,#3975,.F.);
#5615=ORIENTED_EDGE('',*,*,#3976,.T.);
#5616=ORIENTED_EDGE('',*,*,#3972,.T.);
#5617=ORIENTED_EDGE('',*,*,#3977,.F.);
#5618=ORIENTED_EDGE('',*,*,#3978,.F.);
#5619=ORIENTED_EDGE('',*,*,#3979,.T.);
#5620=ORIENTED_EDGE('',*,*,#3975,.T.);
#5621=ORIENTED_EDGE('',*,*,#3980,.F.);
#5622=ORIENTED_EDGE('',*,*,#3981,.F.);
#5623=ORIENTED_EDGE('',*,*,#3982,.T.);
#5624=ORIENTED_EDGE('',*,*,#3978,.T.);
#5625=ORIENTED_EDGE('',*,*,#3983,.F.);
#5626=ORIENTED_EDGE('',*,*,#3984,.F.);
#5627=ORIENTED_EDGE('',*,*,#3985,.T.);
#5628=ORIENTED_EDGE('',*,*,#3981,.T.);
#5629=ORIENTED_EDGE('',*,*,#3986,.F.);
#5630=ORIENTED_EDGE('',*,*,#3987,.F.);
#5631=ORIENTED_EDGE('',*,*,#3988,.T.);
#5632=ORIENTED_EDGE('',*,*,#3984,.T.);
#5633=ORIENTED_EDGE('',*,*,#3989,.F.);
#5634=ORIENTED_EDGE('',*,*,#3990,.F.);
#5635=ORIENTED_EDGE('',*,*,#3991,.T.);
#5636=ORIENTED_EDGE('',*,*,#3987,.T.);
#5637=ORIENTED_EDGE('',*,*,#3992,.F.);
#5638=ORIENTED_EDGE('',*,*,#3993,.F.);
#5639=ORIENTED_EDGE('',*,*,#3994,.T.);
#5640=ORIENTED_EDGE('',*,*,#3990,.T.);
#5641=ORIENTED_EDGE('',*,*,#3995,.F.);
#5642=ORIENTED_EDGE('',*,*,#3996,.F.);
#5643=ORIENTED_EDGE('',*,*,#3997,.T.);
#5644=ORIENTED_EDGE('',*,*,#3993,.T.);
#5645=ORIENTED_EDGE('',*,*,#3998,.F.);
#5646=ORIENTED_EDGE('',*,*,#3999,.F.);
#5647=ORIENTED_EDGE('',*,*,#4000,.T.);
#5648=ORIENTED_EDGE('',*,*,#3996,.T.);
#5649=ORIENTED_EDGE('',*,*,#4001,.F.);
#5650=ORIENTED_EDGE('',*,*,#4002,.F.);
#5651=ORIENTED_EDGE('',*,*,#4003,.T.);
#5652=ORIENTED_EDGE('',*,*,#3999,.T.);
#5653=ORIENTED_EDGE('',*,*,#4004,.F.);
#5654=ORIENTED_EDGE('',*,*,#4005,.F.);
#5655=ORIENTED_EDGE('',*,*,#4006,.T.);
#5656=ORIENTED_EDGE('',*,*,#4002,.T.);
#5657=ORIENTED_EDGE('',*,*,#4007,.F.);
#5658=ORIENTED_EDGE('',*,*,#4008,.F.);
#5659=ORIENTED_EDGE('',*,*,#3919,.F.);
#5660=ORIENTED_EDGE('',*,*,#4009,.F.);
#5661=ORIENTED_EDGE('',*,*,#4010,.F.);
#5662=ORIENTED_EDGE('',*,*,#4011,.F.);
#5663=ORIENTED_EDGE('',*,*,#4012,.T.);
#5664=ORIENTED_EDGE('',*,*,#4013,.F.);
#5665=ORIENTED_EDGE('',*,*,#4012,.F.);
#5666=ORIENTED_EDGE('',*,*,#4009,.T.);
#5667=ORIENTED_EDGE('',*,*,#3918,.F.);
#5668=ORIENTED_EDGE('',*,*,#3922,.F.);
#5669=ORIENTED_EDGE('',*,*,#3925,.F.);
#5670=ORIENTED_EDGE('',*,*,#3928,.F.);
#5671=ORIENTED_EDGE('',*,*,#3931,.F.);
#5672=ORIENTED_EDGE('',*,*,#3934,.F.);
#5673=ORIENTED_EDGE('',*,*,#3937,.F.);
#5674=ORIENTED_EDGE('',*,*,#3940,.F.);
#5675=ORIENTED_EDGE('',*,*,#3943,.F.);
#5676=ORIENTED_EDGE('',*,*,#3946,.F.);
#5677=ORIENTED_EDGE('',*,*,#3949,.F.);
#5678=ORIENTED_EDGE('',*,*,#3952,.F.);
#5679=ORIENTED_EDGE('',*,*,#3955,.F.);
#5680=ORIENTED_EDGE('',*,*,#3958,.F.);
#5681=ORIENTED_EDGE('',*,*,#3961,.F.);
#5682=ORIENTED_EDGE('',*,*,#3964,.F.);
#5683=ORIENTED_EDGE('',*,*,#3967,.F.);
#5684=ORIENTED_EDGE('',*,*,#3970,.F.);
#5685=ORIENTED_EDGE('',*,*,#3973,.F.);
#5686=ORIENTED_EDGE('',*,*,#3976,.F.);
#5687=ORIENTED_EDGE('',*,*,#3979,.F.);
#5688=ORIENTED_EDGE('',*,*,#3982,.F.);
#5689=ORIENTED_EDGE('',*,*,#3985,.F.);
#5690=ORIENTED_EDGE('',*,*,#3988,.F.);
#5691=ORIENTED_EDGE('',*,*,#3991,.F.);
#5692=ORIENTED_EDGE('',*,*,#3994,.F.);
#5693=ORIENTED_EDGE('',*,*,#3997,.F.);
#5694=ORIENTED_EDGE('',*,*,#4000,.F.);
#5695=ORIENTED_EDGE('',*,*,#4003,.F.);
#5696=ORIENTED_EDGE('',*,*,#4006,.F.);
#5697=ORIENTED_EDGE('',*,*,#4014,.F.);
#5698=ORIENTED_EDGE('',*,*,#4015,.F.);
#5699=ORIENTED_EDGE('',*,*,#3827,.F.);
#5700=ORIENTED_EDGE('',*,*,#3831,.F.);
#5701=ORIENTED_EDGE('',*,*,#3834,.F.);
#5702=ORIENTED_EDGE('',*,*,#3837,.F.);
#5703=ORIENTED_EDGE('',*,*,#3840,.F.);
#5704=ORIENTED_EDGE('',*,*,#3843,.F.);
#5705=ORIENTED_EDGE('',*,*,#3846,.F.);
#5706=ORIENTED_EDGE('',*,*,#3849,.F.);
#5707=ORIENTED_EDGE('',*,*,#3852,.F.);
#5708=ORIENTED_EDGE('',*,*,#3855,.F.);
#5709=ORIENTED_EDGE('',*,*,#3858,.F.);
#5710=ORIENTED_EDGE('',*,*,#3861,.F.);
#5711=ORIENTED_EDGE('',*,*,#3864,.F.);
#5712=ORIENTED_EDGE('',*,*,#3867,.F.);
#5713=ORIENTED_EDGE('',*,*,#3870,.F.);
#5714=ORIENTED_EDGE('',*,*,#3873,.F.);
#5715=ORIENTED_EDGE('',*,*,#3876,.F.);
#5716=ORIENTED_EDGE('',*,*,#3879,.F.);
#5717=ORIENTED_EDGE('',*,*,#3882,.F.);
#5718=ORIENTED_EDGE('',*,*,#3885,.F.);
#5719=ORIENTED_EDGE('',*,*,#3888,.F.);
#5720=ORIENTED_EDGE('',*,*,#3891,.F.);
#5721=ORIENTED_EDGE('',*,*,#3894,.F.);
#5722=ORIENTED_EDGE('',*,*,#3897,.F.);
#5723=ORIENTED_EDGE('',*,*,#3900,.F.);
#5724=ORIENTED_EDGE('',*,*,#3903,.F.);
#5725=ORIENTED_EDGE('',*,*,#3906,.F.);
#5726=ORIENTED_EDGE('',*,*,#3909,.F.);
#5727=ORIENTED_EDGE('',*,*,#3912,.F.);
#5728=ORIENTED_EDGE('',*,*,#3915,.F.);
#5729=ORIENTED_EDGE('',*,*,#4016,.F.);
#5730=ORIENTED_EDGE('',*,*,#4005,.T.);
#5731=ORIENTED_EDGE('',*,*,#4017,.F.);
#5732=ORIENTED_EDGE('',*,*,#4018,.F.);
#5733=ORIENTED_EDGE('',*,*,#4014,.T.);
#5734=ORIENTED_EDGE('',*,*,#4008,.T.);
#5735=ORIENTED_EDGE('',*,*,#4011,.T.);
#5736=ORIENTED_EDGE('',*,*,#4019,.F.);
#5737=ORIENTED_EDGE('',*,*,#3916,.F.);
#5738=ORIENTED_EDGE('',*,*,#3913,.F.);
#5739=ORIENTED_EDGE('',*,*,#3910,.F.);
#5740=ORIENTED_EDGE('',*,*,#3907,.F.);
#5741=ORIENTED_EDGE('',*,*,#3904,.F.);
#5742=ORIENTED_EDGE('',*,*,#3901,.F.);
#5743=ORIENTED_EDGE('',*,*,#3898,.F.);
#5744=ORIENTED_EDGE('',*,*,#3895,.F.);
#5745=ORIENTED_EDGE('',*,*,#3892,.F.);
#5746=ORIENTED_EDGE('',*,*,#3889,.F.);
#5747=ORIENTED_EDGE('',*,*,#3886,.F.);
#5748=ORIENTED_EDGE('',*,*,#3883,.F.);
#5749=ORIENTED_EDGE('',*,*,#3880,.F.);
#5750=ORIENTED_EDGE('',*,*,#3877,.F.);
#5751=ORIENTED_EDGE('',*,*,#3874,.F.);
#5752=ORIENTED_EDGE('',*,*,#3871,.F.);
#5753=ORIENTED_EDGE('',*,*,#3868,.F.);
#5754=ORIENTED_EDGE('',*,*,#3865,.F.);
#5755=ORIENTED_EDGE('',*,*,#3862,.F.);
#5756=ORIENTED_EDGE('',*,*,#3859,.F.);
#5757=ORIENTED_EDGE('',*,*,#3856,.F.);
#5758=ORIENTED_EDGE('',*,*,#3853,.F.);
#5759=ORIENTED_EDGE('',*,*,#3850,.F.);
#5760=ORIENTED_EDGE('',*,*,#3847,.F.);
#5761=ORIENTED_EDGE('',*,*,#3844,.F.);
#5762=ORIENTED_EDGE('',*,*,#3841,.F.);
#5763=ORIENTED_EDGE('',*,*,#3838,.F.);
#5764=ORIENTED_EDGE('',*,*,#3835,.F.);
#5765=ORIENTED_EDGE('',*,*,#3832,.F.);
#5766=ORIENTED_EDGE('',*,*,#3829,.F.);
#5767=ORIENTED_EDGE('',*,*,#4020,.F.);
#5768=ORIENTED_EDGE('',*,*,#4017,.T.);
#5769=ORIENTED_EDGE('',*,*,#4007,.T.);
#5770=ORIENTED_EDGE('',*,*,#4004,.T.);
#5771=ORIENTED_EDGE('',*,*,#4001,.T.);
#5772=ORIENTED_EDGE('',*,*,#3998,.T.);
#5773=ORIENTED_EDGE('',*,*,#3995,.T.);
#5774=ORIENTED_EDGE('',*,*,#3992,.T.);
#5775=ORIENTED_EDGE('',*,*,#3989,.T.);
#5776=ORIENTED_EDGE('',*,*,#3986,.T.);
#5777=ORIENTED_EDGE('',*,*,#3983,.T.);
#5778=ORIENTED_EDGE('',*,*,#3980,.T.);
#5779=ORIENTED_EDGE('',*,*,#3977,.T.);
#5780=ORIENTED_EDGE('',*,*,#3974,.T.);
#5781=ORIENTED_EDGE('',*,*,#3971,.T.);
#5782=ORIENTED_EDGE('',*,*,#3968,.T.);
#5783=ORIENTED_EDGE('',*,*,#3965,.T.);
#5784=ORIENTED_EDGE('',*,*,#3962,.T.);
#5785=ORIENTED_EDGE('',*,*,#3959,.T.);
#5786=ORIENTED_EDGE('',*,*,#3956,.T.);
#5787=ORIENTED_EDGE('',*,*,#3953,.T.);
#5788=ORIENTED_EDGE('',*,*,#3950,.T.);
#5789=ORIENTED_EDGE('',*,*,#3947,.T.);
#5790=ORIENTED_EDGE('',*,*,#3944,.T.);
#5791=ORIENTED_EDGE('',*,*,#3941,.T.);
#5792=ORIENTED_EDGE('',*,*,#3938,.T.);
#5793=ORIENTED_EDGE('',*,*,#3935,.T.);
#5794=ORIENTED_EDGE('',*,*,#3932,.T.);
#5795=ORIENTED_EDGE('',*,*,#3929,.T.);
#5796=ORIENTED_EDGE('',*,*,#3926,.T.);
#5797=ORIENTED_EDGE('',*,*,#3923,.T.);
#5798=ORIENTED_EDGE('',*,*,#3920,.T.);
#5799=ORIENTED_EDGE('',*,*,#3914,.T.);
#5800=ORIENTED_EDGE('',*,*,#4019,.T.);
#5801=ORIENTED_EDGE('',*,*,#4010,.T.);
#5802=ORIENTED_EDGE('',*,*,#4016,.T.);
#5803=ORIENTED_EDGE('',*,*,#4021,.F.);
#5804=ORIENTED_EDGE('',*,*,#4022,.T.);
#5805=ORIENTED_EDGE('',*,*,#4023,.T.);
#5806=ORIENTED_EDGE('',*,*,#4024,.F.);
#5807=ORIENTED_EDGE('',*,*,#4025,.F.);
#5808=ORIENTED_EDGE('',*,*,#4026,.T.);
#5809=ORIENTED_EDGE('',*,*,#4027,.T.);
#5810=ORIENTED_EDGE('',*,*,#4022,.F.);
#5811=ORIENTED_EDGE('',*,*,#4028,.F.);
#5812=ORIENTED_EDGE('',*,*,#4029,.T.);
#5813=ORIENTED_EDGE('',*,*,#4030,.T.);
#5814=ORIENTED_EDGE('',*,*,#4026,.F.);
#5815=ORIENTED_EDGE('',*,*,#4031,.F.);
#5816=ORIENTED_EDGE('',*,*,#4032,.T.);
#5817=ORIENTED_EDGE('',*,*,#4033,.T.);
#5818=ORIENTED_EDGE('',*,*,#4029,.F.);
#5819=ORIENTED_EDGE('',*,*,#4034,.F.);
#5820=ORIENTED_EDGE('',*,*,#4035,.T.);
#5821=ORIENTED_EDGE('',*,*,#4036,.T.);
#5822=ORIENTED_EDGE('',*,*,#4032,.F.);
#5823=ORIENTED_EDGE('',*,*,#4037,.F.);
#5824=ORIENTED_EDGE('',*,*,#4024,.T.);
#5825=ORIENTED_EDGE('',*,*,#4038,.T.);
#5826=ORIENTED_EDGE('',*,*,#4035,.F.);
#5827=ORIENTED_EDGE('',*,*,#4038,.F.);
#5828=ORIENTED_EDGE('',*,*,#4023,.F.);
#5829=ORIENTED_EDGE('',*,*,#4027,.F.);
#5830=ORIENTED_EDGE('',*,*,#4030,.F.);
#5831=ORIENTED_EDGE('',*,*,#4033,.F.);
#5832=ORIENTED_EDGE('',*,*,#4036,.F.);
#5833=ORIENTED_EDGE('',*,*,#4039,.T.);
#5834=ORIENTED_EDGE('',*,*,#4015,.T.);
#5835=ORIENTED_EDGE('',*,*,#4018,.T.);
#5836=ORIENTED_EDGE('',*,*,#4020,.T.);
#5837=ORIENTED_EDGE('',*,*,#3828,.F.);
#5838=ORIENTED_EDGE('',*,*,#4039,.F.);
#5839=ORIENTED_EDGE('',*,*,#4040,.T.);
#5840=ORIENTED_EDGE('',*,*,#4041,.T.);
#5841=ORIENTED_EDGE('',*,*,#4040,.F.);
#5842=ORIENTED_EDGE('',*,*,#4041,.F.);
#5843=ORIENTED_EDGE('',*,*,#4021,.T.);
#5844=ORIENTED_EDGE('',*,*,#4037,.T.);
#5845=ORIENTED_EDGE('',*,*,#4034,.T.);
#5846=ORIENTED_EDGE('',*,*,#4031,.T.);
#5847=ORIENTED_EDGE('',*,*,#4028,.T.);
#5848=ORIENTED_EDGE('',*,*,#4025,.T.);
#5849=ORIENTED_EDGE('',*,*,#4013,.T.);
#5850=ORIENTED_EDGE('',*,*,#4042,.T.);
#5851=ORIENTED_EDGE('',*,*,#4043,.F.);
#5852=ORIENTED_EDGE('',*,*,#4044,.T.);
#5853=ORIENTED_EDGE('',*,*,#4045,.T.);
#5854=ORIENTED_EDGE('',*,*,#4046,.T.);
#5855=ORIENTED_EDGE('',*,*,#4047,.F.);
#5856=ORIENTED_EDGE('',*,*,#4042,.F.);
#5857=ORIENTED_EDGE('',*,*,#4048,.T.);
#5858=ORIENTED_EDGE('',*,*,#4049,.T.);
#5859=ORIENTED_EDGE('',*,*,#4050,.T.);
#5860=ORIENTED_EDGE('',*,*,#4045,.F.);
#5861=ORIENTED_EDGE('',*,*,#4051,.T.);
#5862=ORIENTED_EDGE('',*,*,#4052,.T.);
#5863=ORIENTED_EDGE('',*,*,#4053,.T.);
#5864=ORIENTED_EDGE('',*,*,#4049,.F.);
#5865=ORIENTED_EDGE('',*,*,#4054,.T.);
#5866=ORIENTED_EDGE('',*,*,#4055,.F.);
#5867=ORIENTED_EDGE('',*,*,#4056,.T.);
#5868=ORIENTED_EDGE('',*,*,#4057,.F.);
#5869=ORIENTED_EDGE('',*,*,#4058,.T.);
#5870=ORIENTED_EDGE('',*,*,#4059,.T.);
#5871=ORIENTED_EDGE('',*,*,#4060,.T.);
#5872=ORIENTED_EDGE('',*,*,#4061,.F.);
#5873=ORIENTED_EDGE('',*,*,#4062,.F.);
#5874=ORIENTED_EDGE('',*,*,#4063,.T.);
#5875=ORIENTED_EDGE('',*,*,#4064,.T.);
#5876=ORIENTED_EDGE('',*,*,#4059,.F.);
#5877=ORIENTED_EDGE('',*,*,#4065,.F.);
#5878=ORIENTED_EDGE('',*,*,#4066,.T.);
#5879=ORIENTED_EDGE('',*,*,#4067,.T.);
#5880=ORIENTED_EDGE('',*,*,#4063,.F.);
#5881=ORIENTED_EDGE('',*,*,#4068,.F.);
#5882=ORIENTED_EDGE('',*,*,#4069,.T.);
#5883=ORIENTED_EDGE('',*,*,#4070,.T.);
#5884=ORIENTED_EDGE('',*,*,#4066,.F.);
#5885=ORIENTED_EDGE('',*,*,#4071,.F.);
#5886=ORIENTED_EDGE('',*,*,#4072,.F.);
#5887=ORIENTED_EDGE('',*,*,#4073,.F.);
#5888=ORIENTED_EDGE('',*,*,#4074,.F.);
#5889=ORIENTED_EDGE('',*,*,#4075,.T.);
#5890=ORIENTED_EDGE('',*,*,#4072,.T.);
#5891=ORIENTED_EDGE('',*,*,#4076,.T.);
#5892=ORIENTED_EDGE('',*,*,#4069,.F.);
#5893=ORIENTED_EDGE('',*,*,#4077,.F.);
#5894=ORIENTED_EDGE('',*,*,#4078,.F.);
#5895=ORIENTED_EDGE('',*,*,#4060,.F.);
#5896=ORIENTED_EDGE('',*,*,#4064,.F.);
#5897=ORIENTED_EDGE('',*,*,#4067,.F.);
#5898=ORIENTED_EDGE('',*,*,#4070,.F.);
#5899=ORIENTED_EDGE('',*,*,#4076,.F.);
#5900=ORIENTED_EDGE('',*,*,#4075,.F.);
#5901=ORIENTED_EDGE('',*,*,#4079,.F.);
#5902=ORIENTED_EDGE('',*,*,#4056,.F.);
#5903=ORIENTED_EDGE('',*,*,#4080,.F.);
#5904=ORIENTED_EDGE('',*,*,#4054,.F.);
#5905=ORIENTED_EDGE('',*,*,#4051,.F.);
#5906=ORIENTED_EDGE('',*,*,#4048,.F.);
#5907=ORIENTED_EDGE('',*,*,#4044,.F.);
#5908=ORIENTED_EDGE('',*,*,#4081,.F.);
#5909=ORIENTED_EDGE('',*,*,#4046,.F.);
#5910=ORIENTED_EDGE('',*,*,#4050,.F.);
#5911=ORIENTED_EDGE('',*,*,#4053,.F.);
#5912=ORIENTED_EDGE('',*,*,#4082,.F.);
#5913=ORIENTED_EDGE('',*,*,#4058,.F.);
#5914=ORIENTED_EDGE('',*,*,#4083,.F.);
#5915=ORIENTED_EDGE('',*,*,#4073,.T.);
#5916=ORIENTED_EDGE('',*,*,#4077,.T.);
#5917=ORIENTED_EDGE('',*,*,#4071,.T.);
#5918=ORIENTED_EDGE('',*,*,#4068,.T.);
#5919=ORIENTED_EDGE('',*,*,#4065,.T.);
#5920=ORIENTED_EDGE('',*,*,#4062,.T.);
#5921=ORIENTED_EDGE('',*,*,#4084,.T.);
#5922=ORIENTED_EDGE('',*,*,#4085,.T.);
#5923=ORIENTED_EDGE('',*,*,#4086,.T.);
#5924=ORIENTED_EDGE('',*,*,#4087,.T.);
#5925=ORIENTED_EDGE('',*,*,#4088,.T.);
#5926=ORIENTED_EDGE('',*,*,#4089,.T.);
#5927=ORIENTED_EDGE('',*,*,#4079,.T.);
#5928=ORIENTED_EDGE('',*,*,#4074,.T.);
#5929=ORIENTED_EDGE('',*,*,#4083,.T.);
#5930=ORIENTED_EDGE('',*,*,#4057,.T.);
#5931=ORIENTED_EDGE('',*,*,#4055,.T.);
#5932=ORIENTED_EDGE('',*,*,#4082,.T.);
#5933=ORIENTED_EDGE('',*,*,#4052,.F.);
#5934=ORIENTED_EDGE('',*,*,#4080,.T.);
#5935=ORIENTED_EDGE('',*,*,#4090,.T.);
#5936=ORIENTED_EDGE('',*,*,#4091,.T.);
#5937=ORIENTED_EDGE('',*,*,#4089,.F.);
#5938=ORIENTED_EDGE('',*,*,#4092,.F.);
#5939=ORIENTED_EDGE('',*,*,#4093,.T.);
#5940=ORIENTED_EDGE('',*,*,#4092,.T.);
#5941=ORIENTED_EDGE('',*,*,#4088,.F.);
#5942=ORIENTED_EDGE('',*,*,#4094,.F.);
#5943=ORIENTED_EDGE('',*,*,#4095,.T.);
#5944=ORIENTED_EDGE('',*,*,#4094,.T.);
#5945=ORIENTED_EDGE('',*,*,#4087,.F.);
#5946=ORIENTED_EDGE('',*,*,#4096,.F.);
#5947=ORIENTED_EDGE('',*,*,#4097,.T.);
#5948=ORIENTED_EDGE('',*,*,#4096,.T.);
#5949=ORIENTED_EDGE('',*,*,#4086,.F.);
#5950=ORIENTED_EDGE('',*,*,#4098,.F.);
#5951=ORIENTED_EDGE('',*,*,#4099,.T.);
#5952=ORIENTED_EDGE('',*,*,#4098,.T.);
#5953=ORIENTED_EDGE('',*,*,#4085,.F.);
#5954=ORIENTED_EDGE('',*,*,#4100,.F.);
#5955=ORIENTED_EDGE('',*,*,#4101,.T.);
#5956=ORIENTED_EDGE('',*,*,#4100,.T.);
#5957=ORIENTED_EDGE('',*,*,#4084,.F.);
#5958=ORIENTED_EDGE('',*,*,#4091,.F.);
#5959=ORIENTED_EDGE('',*,*,#4101,.F.);
#5960=ORIENTED_EDGE('',*,*,#4090,.F.);
#5961=ORIENTED_EDGE('',*,*,#4093,.F.);
#5962=ORIENTED_EDGE('',*,*,#4095,.F.);
#5963=ORIENTED_EDGE('',*,*,#4097,.F.);
#5964=ORIENTED_EDGE('',*,*,#4099,.F.);
#5965=ORIENTED_EDGE('',*,*,#4078,.T.);
#5966=ORIENTED_EDGE('',*,*,#4043,.T.);
#5967=ORIENTED_EDGE('',*,*,#4047,.T.);
#5968=ORIENTED_EDGE('',*,*,#4081,.T.);
#5969=ORIENTED_EDGE('',*,*,#4061,.T.);
#5970=ORIENTED_EDGE('',*,*,#4102,.F.);
#5971=ORIENTED_EDGE('',*,*,#4103,.T.);
#5972=ORIENTED_EDGE('',*,*,#4104,.T.);
#5973=ORIENTED_EDGE('',*,*,#4103,.F.);
#5974=ORIENTED_EDGE('',*,*,#4105,.F.);
#5975=ORIENTED_EDGE('',*,*,#4106,.T.);
#5976=ORIENTED_EDGE('',*,*,#4107,.T.);
#5977=ORIENTED_EDGE('',*,*,#4106,.F.);
#5978=ORIENTED_EDGE('',*,*,#4105,.T.);
#5979=ORIENTED_EDGE('',*,*,#4102,.T.);
#5980=ORIENTED_EDGE('',*,*,#4107,.F.);
#5981=ORIENTED_EDGE('',*,*,#4104,.F.);
#5982=CYLINDRICAL_SURFACE('',#6597,0.17);
#5983=CYLINDRICAL_SURFACE('',#6600,0.17);
#5984=CYLINDRICAL_SURFACE('',#6603,0.41);
#5985=CYLINDRICAL_SURFACE('',#6613,0.2);
#5986=CYLINDRICAL_SURFACE('',#6616,12.0894198846614);
#5987=CYLINDRICAL_SURFACE('',#6624,1.4);
#5988=CYLINDRICAL_SURFACE('',#6627,1.4);
#5989=CYLINDRICAL_SURFACE('',#6638,1.1);
#5990=CYLINDRICAL_SURFACE('',#6646,1.7);
#5991=CYLINDRICAL_SURFACE('',#6647,1.7);
#5992=CYLINDRICAL_SURFACE('',#6657,0.3);
#5993=CYLINDRICAL_SURFACE('',#6664,0.4);
#5994=CYLINDRICAL_SURFACE('',#6669,0.6);
#5995=CYLINDRICAL_SURFACE('',#6672,0.4);
#5996=CYLINDRICAL_SURFACE('',#6680,0.3);
#5997=CYLINDRICAL_SURFACE('',#6682,0.6);
#5998=CYLINDRICAL_SURFACE('',#6687,0.15);
#5999=CYLINDRICAL_SURFACE('',#6690,0.15);
#6000=CYLINDRICAL_SURFACE('',#6693,0.15);
#6001=CYLINDRICAL_SURFACE('',#6696,0.15);
#6002=CYLINDRICAL_SURFACE('',#6699,0.3);
#6003=CYLINDRICAL_SURFACE('',#6704,0.3);
#6004=CYLINDRICAL_SURFACE('',#6709,0.17);
#6005=CYLINDRICAL_SURFACE('',#6711,0.17);
#6006=CYLINDRICAL_SURFACE('',#6735,0.4);
#6007=CYLINDRICAL_SURFACE('',#6737,0.4);
#6008=CYLINDRICAL_SURFACE('',#6761,0.1);
#6009=CYLINDRICAL_SURFACE('',#6765,0.1);
#6010=CYLINDRICAL_SURFACE('',#6779,0.3);
#6011=CYLINDRICAL_SURFACE('',#6784,0.3);
#6012=CYLINDRICAL_SURFACE('',#6789,0.15);
#6013=CYLINDRICAL_SURFACE('',#6792,0.15);
#6014=CYLINDRICAL_SURFACE('',#6795,0.15);
#6015=CYLINDRICAL_SURFACE('',#6798,0.15);
#6016=CYLINDRICAL_SURFACE('',#6817,0.17);
#6017=CYLINDRICAL_SURFACE('',#6819,0.17);
#6018=CYLINDRICAL_SURFACE('',#6843,0.4);
#6019=CYLINDRICAL_SURFACE('',#6845,0.4);
#6020=CYLINDRICAL_SURFACE('',#6869,0.1);
#6021=CYLINDRICAL_SURFACE('',#6873,0.1);
#6022=CYLINDRICAL_SURFACE('',#6887,0.3);
#6023=CYLINDRICAL_SURFACE('',#6892,0.3);
#6024=CYLINDRICAL_SURFACE('',#6897,0.35);
#6025=CYLINDRICAL_SURFACE('',#6900,0.35);
#6026=CYLINDRICAL_SURFACE('',#6906,0.25);
#6027=CYLINDRICAL_SURFACE('',#6912,0.25);
#6028=CYLINDRICAL_SURFACE('',#6918,0.25);
#6029=CYLINDRICAL_SURFACE('',#6924,0.25);
#6030=CYLINDRICAL_SURFACE('',#6927,0.15);
#6031=CYLINDRICAL_SURFACE('',#6929,0.15);
#6032=CYLINDRICAL_SURFACE('',#6931,0.15);
#6033=CYLINDRICAL_SURFACE('',#6933,0.15);
#6034=CYLINDRICAL_SURFACE('',#6937,0.08);
#6035=CYLINDRICAL_SURFACE('',#6942,0.08);
#6036=CYLINDRICAL_SURFACE('',#6950,0.14635);
#6037=CYLINDRICAL_SURFACE('',#6952,0.14635);
#6038=CYLINDRICAL_SURFACE('',#6953,0.14635);
#6039=CYLINDRICAL_SURFACE('',#6954,0.14635);
#6040=CYLINDRICAL_SURFACE('',#6955,0.14635);
#6041=CYLINDRICAL_SURFACE('',#6956,0.14635);
#6042=CYLINDRICAL_SURFACE('',#6957,0.14635);
#6043=CYLINDRICAL_SURFACE('',#6958,0.14635);
#6044=CYLINDRICAL_SURFACE('',#6959,0.14635);
#6045=CYLINDRICAL_SURFACE('',#6960,0.14635);
#6046=CYLINDRICAL_SURFACE('',#6961,0.14635);
#6047=CYLINDRICAL_SURFACE('',#6962,0.14635);
#6048=CYLINDRICAL_SURFACE('',#6963,0.14635);
#6049=CYLINDRICAL_SURFACE('',#6964,0.14635);
#6050=CYLINDRICAL_SURFACE('',#6965,0.14635);
#6051=CYLINDRICAL_SURFACE('',#6966,0.14635);
#6052=CYLINDRICAL_SURFACE('',#6967,0.14635);
#6053=CYLINDRICAL_SURFACE('',#6968,0.14635);
#6054=CYLINDRICAL_SURFACE('',#6969,0.14635);
#6055=CYLINDRICAL_SURFACE('',#6970,0.14635);
#6056=CYLINDRICAL_SURFACE('',#6971,0.14635);
#6057=CYLINDRICAL_SURFACE('',#6972,0.14635);
#6058=CYLINDRICAL_SURFACE('',#6973,0.14635);
#6059=CYLINDRICAL_SURFACE('',#6974,0.14635);
#6060=CYLINDRICAL_SURFACE('',#6975,0.14635);
#6061=CYLINDRICAL_SURFACE('',#6976,0.14635);
#6062=CYLINDRICAL_SURFACE('',#6977,0.14635);
#6063=CYLINDRICAL_SURFACE('',#6978,0.14635);
#6064=CYLINDRICAL_SURFACE('',#6979,0.14635);
#6065=CYLINDRICAL_SURFACE('',#6980,0.14635);
#6066=CYLINDRICAL_SURFACE('',#6981,0.117775);
#6067=CYLINDRICAL_SURFACE('',#6983,0.117775);
#6068=CYLINDRICAL_SURFACE('',#6984,0.117775);
#6069=CYLINDRICAL_SURFACE('',#6985,0.117775);
#6070=CYLINDRICAL_SURFACE('',#6986,0.117775);
#6071=CYLINDRICAL_SURFACE('',#6987,0.117775);
#6072=CYLINDRICAL_SURFACE('',#6988,0.117775);
#6073=CYLINDRICAL_SURFACE('',#6989,0.117775);
#6074=CYLINDRICAL_SURFACE('',#6990,0.117775);
#6075=CYLINDRICAL_SURFACE('',#6991,0.117775);
#6076=CYLINDRICAL_SURFACE('',#6992,0.117775);
#6077=CYLINDRICAL_SURFACE('',#6993,0.117775);
#6078=CYLINDRICAL_SURFACE('',#6994,0.117775);
#6079=CYLINDRICAL_SURFACE('',#6995,0.117775);
#6080=CYLINDRICAL_SURFACE('',#6996,0.117775);
#6081=CYLINDRICAL_SURFACE('',#6997,0.117775);
#6082=CYLINDRICAL_SURFACE('',#6998,0.117775);
#6083=CYLINDRICAL_SURFACE('',#6999,0.117775);
#6084=CYLINDRICAL_SURFACE('',#7000,0.117775);
#6085=CYLINDRICAL_SURFACE('',#7001,0.117775);
#6086=CYLINDRICAL_SURFACE('',#7002,0.117775);
#6087=CYLINDRICAL_SURFACE('',#7003,0.117775);
#6088=CYLINDRICAL_SURFACE('',#7004,0.117775);
#6089=CYLINDRICAL_SURFACE('',#7005,0.117775);
#6090=CYLINDRICAL_SURFACE('',#7006,0.117775);
#6091=CYLINDRICAL_SURFACE('',#7007,0.117775);
#6092=CYLINDRICAL_SURFACE('',#7008,0.117775);
#6093=CYLINDRICAL_SURFACE('',#7009,0.117775);
#6094=CYLINDRICAL_SURFACE('',#7010,0.117775);
#6095=CYLINDRICAL_SURFACE('',#7011,0.117775);
#6096=CYLINDRICAL_SURFACE('',#7015,0.117775);
#6097=CYLINDRICAL_SURFACE('',#7017,0.14635);
#6098=CYLINDRICAL_SURFACE('',#7027,0.275);
#6099=CYLINDRICAL_SURFACE('',#7032,0.12645);
#6100=CYLINDRICAL_SURFACE('',#7034,0.12645);
#6101=CYLINDRICAL_SURFACE('',#7036,0.12645);
#6102=CYLINDRICAL_SURFACE('',#7037,0.12645);
#6103=CYLINDRICAL_SURFACE('',#7038,0.12645);
#6104=CYLINDRICAL_SURFACE('',#7040,0.1543);
#6105=CYLINDRICAL_SURFACE('',#7042,0.1543);
#6106=CYLINDRICAL_SURFACE('',#7043,0.1543);
#6107=CYLINDRICAL_SURFACE('',#7044,0.1543);
#6108=CYLINDRICAL_SURFACE('',#7045,0.1543);
#6109=CYLINDRICAL_SURFACE('',#7047,0.1543);
#6110=CYLINDRICAL_SURFACE('',#7049,0.12645);
#6111=CYLINDRICAL_SURFACE('',#7066,0.41);
#6112=CYLINDRICAL_SURFACE('',#7069,0.6);
#6113=ADVANCED_FACE('',(#782),#5982,.F.);
#6114=ADVANCED_FACE('',(#783),#5983,.F.);
#6115=ADVANCED_FACE('',(#784),#5984,.F.);
#6116=ADVANCED_FACE('',(#785),#640,.F.);
#6117=ADVANCED_FACE('',(#786),#638,.T.);
#6118=ADVANCED_FACE('',(#787),#641,.T.);
#6119=ADVANCED_FACE('',(#788),#642,.T.);
#6120=ADVANCED_FACE('',(#789),#643,.T.);
#6121=ADVANCED_FACE('',(#790),#5985,.T.);
#6122=ADVANCED_FACE('',(#791),#5986,.T.);
#6123=ADVANCED_FACE('',(#792),#644,.T.);
#6124=ADVANCED_FACE('',(#793),#645,.T.);
#6125=ADVANCED_FACE('',(#794),#646,.T.);
#6126=ADVANCED_FACE('',(#795),#647,.T.);
#6127=ADVANCED_FACE('',(#796),#648,.T.);
#6128=ADVANCED_FACE('',(#797),#5987,.T.);
#6129=ADVANCED_FACE('',(#798),#5988,.T.);
#6130=ADVANCED_FACE('',(#799,#575,#576,#577,#578),#649,.T.);
#6131=ADVANCED_FACE('',(#800),#573,.T.);
#6132=ADVANCED_FACE('',(#801),#5989,.F.);
#6133=ADVANCED_FACE('',(#802,#579,#580,#581,#582),#650,.F.);
#6134=ADVANCED_FACE('',(#803),#574,.T.);
#6135=ADVANCED_FACE('',(#804),#5990,.T.);
#6136=ADVANCED_FACE('',(#805),#5991,.T.);
#6137=ADVANCED_FACE('',(#806),#651,.T.);
#6138=ADVANCED_FACE('',(#807),#652,.T.);
#6139=ADVANCED_FACE('',(#808),#653,.T.);
#6140=ADVANCED_FACE('',(#809),#654,.T.);
#6141=ADVANCED_FACE('',(#810),#655,.T.);
#6142=ADVANCED_FACE('',(#811),#656,.T.);
#6143=ADVANCED_FACE('',(#812),#657,.T.);
#6144=ADVANCED_FACE('',(#813),#658,.T.);
#6145=ADVANCED_FACE('',(#814),#5992,.T.);
#6146=ADVANCED_FACE('',(#815,#583),#659,.F.);
#6147=ADVANCED_FACE('',(#816,#584),#660,.F.);
#6148=ADVANCED_FACE('',(#817),#5993,.T.);
#6149=ADVANCED_FACE('',(#818,#585),#661,.T.);
#6150=ADVANCED_FACE('',(#819),#5994,.T.);
#6151=ADVANCED_FACE('',(#820),#662,.F.);
#6152=ADVANCED_FACE('',(#821),#5995,.T.);
#6153=ADVANCED_FACE('',(#822),#663,.T.);
#6154=ADVANCED_FACE('',(#823),#664,.F.);
#6155=ADVANCED_FACE('',(#824),#665,.F.);
#6156=ADVANCED_FACE('',(#825),#666,.F.);
#6157=ADVANCED_FACE('',(#826),#5996,.F.);
#6158=ADVANCED_FACE('',(#827),#5997,.T.);
#6159=ADVANCED_FACE('',(#828),#667,.T.);
#6160=ADVANCED_FACE('',(#829),#5998,.F.);
#6161=ADVANCED_FACE('',(#830),#5999,.F.);
#6162=ADVANCED_FACE('',(#831),#6000,.F.);
#6163=ADVANCED_FACE('',(#832),#6001,.F.);
#6164=ADVANCED_FACE('',(#833),#6002,.F.);
#6165=ADVANCED_FACE('',(#834,#586),#668,.F.);
#6166=ADVANCED_FACE('',(#835),#6003,.F.);
#6167=ADVANCED_FACE('',(#836,#587),#669,.F.);
#6168=ADVANCED_FACE('',(#837),#6004,.F.);
#6169=ADVANCED_FACE('',(#838),#6005,.F.);
#6170=ADVANCED_FACE('',(#839),#670,.F.);
#6171=ADVANCED_FACE('',(#840),#671,.F.);
#6172=ADVANCED_FACE('',(#841),#672,.F.);
#6173=ADVANCED_FACE('',(#842),#673,.F.);
#6174=ADVANCED_FACE('',(#843),#674,.F.);
#6175=ADVANCED_FACE('',(#844),#675,.F.);
#6176=ADVANCED_FACE('',(#845),#676,.F.);
#6177=ADVANCED_FACE('',(#846,#588),#677,.F.);
#6178=ADVANCED_FACE('',(#847,#589),#678,.F.);
#6179=ADVANCED_FACE('',(#848),#679,.F.);
#6180=ADVANCED_FACE('',(#849),#680,.F.);
#6181=ADVANCED_FACE('',(#850),#681,.F.);
#6182=ADVANCED_FACE('',(#851),#682,.F.);
#6183=ADVANCED_FACE('',(#852),#683,.F.);
#6184=ADVANCED_FACE('',(#853),#684,.T.);
#6185=ADVANCED_FACE('',(#854),#685,.T.);
#6186=ADVANCED_FACE('',(#855),#686,.T.);
#6187=ADVANCED_FACE('',(#856),#687,.T.);
#6188=ADVANCED_FACE('',(#857),#688,.T.);
#6189=ADVANCED_FACE('',(#858,#590),#689,.F.);
#6190=ADVANCED_FACE('',(#859),#6006,.T.);
#6191=ADVANCED_FACE('',(#860),#6007,.T.);
#6192=ADVANCED_FACE('',(#861),#690,.T.);
#6193=ADVANCED_FACE('',(#862),#91,.T.);
#6194=ADVANCED_FACE('',(#863),#92,.T.);
#6195=ADVANCED_FACE('',(#864),#93,.T.);
#6196=ADVANCED_FACE('',(#865),#94,.T.);
#6197=ADVANCED_FACE('',(#866,#591,#592,#593),#691,.F.);
#6198=ADVANCED_FACE('',(#867),#692,.F.);
#6199=ADVANCED_FACE('',(#868),#95,.T.);
#6200=ADVANCED_FACE('',(#869),#96,.T.);
#6201=ADVANCED_FACE('',(#870),#97,.T.);
#6202=ADVANCED_FACE('',(#871),#693,.T.);
#6203=ADVANCED_FACE('',(#872),#98,.T.);
#6204=ADVANCED_FACE('',(#873),#99,.T.);
#6205=ADVANCED_FACE('',(#874),#694,.F.);
#6206=ADVANCED_FACE('',(#875),#100,.T.);
#6207=ADVANCED_FACE('',(#876),#101,.T.);
#6208=ADVANCED_FACE('',(#877),#695,.T.);
#6209=ADVANCED_FACE('',(#878),#102,.T.);
#6210=ADVANCED_FACE('',(#879),#103,.T.);
#6211=ADVANCED_FACE('',(#880,#594,#595,#596),#696,.F.);
#6212=ADVANCED_FACE('',(#881),#104,.T.);
#6213=ADVANCED_FACE('',(#882),#105,.T.);
#6214=ADVANCED_FACE('',(#883),#697,.T.);
#6215=ADVANCED_FACE('',(#884),#106,.T.);
#6216=ADVANCED_FACE('',(#885),#107,.T.);
#6217=ADVANCED_FACE('',(#886),#698,.F.);
#6218=ADVANCED_FACE('',(#887),#108,.T.);
#6219=ADVANCED_FACE('',(#888),#109,.T.);
#6220=ADVANCED_FACE('',(#889),#75,.F.);
#6221=ADVANCED_FACE('',(#890),#76,.F.);
#6222=ADVANCED_FACE('',(#891),#77,.F.);
#6223=ADVANCED_FACE('',(#892),#6008,.F.);
#6224=ADVANCED_FACE('',(#893),#110,.T.);
#6225=ADVANCED_FACE('',(#894),#78,.F.);
#6226=ADVANCED_FACE('',(#895),#6009,.F.);
#6227=ADVANCED_FACE('',(#896),#111,.T.);
#6228=ADVANCED_FACE('',(#897),#112,.T.);
#6229=ADVANCED_FACE('',(#898),#113,.T.);
#6230=ADVANCED_FACE('',(#899),#114,.T.);
#6231=ADVANCED_FACE('',(#900),#699,.T.);
#6232=ADVANCED_FACE('',(#901),#79,.T.);
#6233=ADVANCED_FACE('',(#902),#80,.T.);
#6234=ADVANCED_FACE('',(#903),#81,.T.);
#6235=ADVANCED_FACE('',(#904),#6010,.T.);
#6236=ADVANCED_FACE('',(#905),#115,.F.);
#6237=ADVANCED_FACE('',(#906),#82,.T.);
#6238=ADVANCED_FACE('',(#907),#6011,.T.);
#6239=ADVANCED_FACE('',(#908),#116,.F.);
#6240=ADVANCED_FACE('',(#909),#117,.F.);
#6241=ADVANCED_FACE('',(#910),#118,.F.);
#6242=ADVANCED_FACE('',(#911),#119,.F.);
#6243=ADVANCED_FACE('',(#912),#120,.F.);
#6244=ADVANCED_FACE('',(#913),#121,.F.);
#6245=ADVANCED_FACE('',(#914),#700,.F.);
#6246=ADVANCED_FACE('',(#915,#597,#598,#599,#600,#601,#602),#701,.T.);
#6247=ADVANCED_FACE('',(#916),#122,.F.);
#6248=ADVANCED_FACE('',(#917),#702,.F.);
#6249=ADVANCED_FACE('',(#918),#6012,.F.);
#6250=ADVANCED_FACE('',(#919),#6013,.F.);
#6251=ADVANCED_FACE('',(#920),#6014,.F.);
#6252=ADVANCED_FACE('',(#921),#6015,.F.);
#6253=ADVANCED_FACE('',(#922),#703,.F.);
#6254=ADVANCED_FACE('',(#923),#704,.F.);
#6255=ADVANCED_FACE('',(#924),#705,.F.);
#6256=ADVANCED_FACE('',(#925),#706,.F.);
#6257=ADVANCED_FACE('',(#926),#707,.F.);
#6258=ADVANCED_FACE('',(#927),#708,.F.);
#6259=ADVANCED_FACE('',(#928,#603),#709,.F.);
#6260=ADVANCED_FACE('',(#929),#710,.F.);
#6261=ADVANCED_FACE('',(#930),#711,.F.);
#6262=ADVANCED_FACE('',(#931),#712,.F.);
#6263=ADVANCED_FACE('',(#932),#713,.F.);
#6264=ADVANCED_FACE('',(#933),#714,.F.);
#6265=ADVANCED_FACE('',(#934),#715,.F.);
#6266=ADVANCED_FACE('',(#935,#604),#716,.F.);
#6267=ADVANCED_FACE('',(#936),#6016,.F.);
#6268=ADVANCED_FACE('',(#937),#6017,.F.);
#6269=ADVANCED_FACE('',(#938),#717,.F.);
#6270=ADVANCED_FACE('',(#939),#718,.F.);
#6271=ADVANCED_FACE('',(#940),#719,.F.);
#6272=ADVANCED_FACE('',(#941),#720,.F.);
#6273=ADVANCED_FACE('',(#942),#721,.F.);
#6274=ADVANCED_FACE('',(#943),#722,.F.);
#6275=ADVANCED_FACE('',(#944),#723,.F.);
#6276=ADVANCED_FACE('',(#945,#605),#724,.F.);
#6277=ADVANCED_FACE('',(#946,#606),#725,.F.);
#6278=ADVANCED_FACE('',(#947),#726,.F.);
#6279=ADVANCED_FACE('',(#948),#727,.F.);
#6280=ADVANCED_FACE('',(#949),#728,.F.);
#6281=ADVANCED_FACE('',(#950),#729,.F.);
#6282=ADVANCED_FACE('',(#951),#730,.F.);
#6283=ADVANCED_FACE('',(#952),#731,.T.);
#6284=ADVANCED_FACE('',(#953),#732,.T.);
#6285=ADVANCED_FACE('',(#954),#733,.T.);
#6286=ADVANCED_FACE('',(#955),#734,.T.);
#6287=ADVANCED_FACE('',(#956),#735,.T.);
#6288=ADVANCED_FACE('',(#957,#607),#736,.F.);
#6289=ADVANCED_FACE('',(#958),#6018,.T.);
#6290=ADVANCED_FACE('',(#959),#6019,.T.);
#6291=ADVANCED_FACE('',(#960),#737,.T.);
#6292=ADVANCED_FACE('',(#961),#123,.T.);
#6293=ADVANCED_FACE('',(#962),#124,.T.);
#6294=ADVANCED_FACE('',(#963),#125,.T.);
#6295=ADVANCED_FACE('',(#964),#126,.T.);
#6296=ADVANCED_FACE('',(#965,#608,#609,#610),#738,.F.);
#6297=ADVANCED_FACE('',(#966),#739,.F.);
#6298=ADVANCED_FACE('',(#967),#127,.T.);
#6299=ADVANCED_FACE('',(#968),#128,.T.);
#6300=ADVANCED_FACE('',(#969),#129,.T.);
#6301=ADVANCED_FACE('',(#970),#740,.T.);
#6302=ADVANCED_FACE('',(#971),#130,.T.);
#6303=ADVANCED_FACE('',(#972),#131,.T.);
#6304=ADVANCED_FACE('',(#973),#741,.F.);
#6305=ADVANCED_FACE('',(#974),#132,.T.);
#6306=ADVANCED_FACE('',(#975),#133,.T.);
#6307=ADVANCED_FACE('',(#976),#742,.T.);
#6308=ADVANCED_FACE('',(#977),#134,.T.);
#6309=ADVANCED_FACE('',(#978),#135,.T.);
#6310=ADVANCED_FACE('',(#979,#611,#612,#613),#743,.F.);
#6311=ADVANCED_FACE('',(#980),#136,.T.);
#6312=ADVANCED_FACE('',(#981),#137,.T.);
#6313=ADVANCED_FACE('',(#982),#744,.T.);
#6314=ADVANCED_FACE('',(#983),#138,.T.);
#6315=ADVANCED_FACE('',(#984),#139,.T.);
#6316=ADVANCED_FACE('',(#985),#745,.F.);
#6317=ADVANCED_FACE('',(#986),#140,.T.);
#6318=ADVANCED_FACE('',(#987),#141,.T.);
#6319=ADVANCED_FACE('',(#988),#83,.F.);
#6320=ADVANCED_FACE('',(#989),#84,.F.);
#6321=ADVANCED_FACE('',(#990),#85,.F.);
#6322=ADVANCED_FACE('',(#991),#6020,.F.);
#6323=ADVANCED_FACE('',(#992),#142,.T.);
#6324=ADVANCED_FACE('',(#993),#86,.F.);
#6325=ADVANCED_FACE('',(#994),#6021,.F.);
#6326=ADVANCED_FACE('',(#995),#143,.T.);
#6327=ADVANCED_FACE('',(#996),#144,.T.);
#6328=ADVANCED_FACE('',(#997),#145,.T.);
#6329=ADVANCED_FACE('',(#998),#146,.T.);
#6330=ADVANCED_FACE('',(#999),#746,.T.);
#6331=ADVANCED_FACE('',(#1000),#87,.T.);
#6332=ADVANCED_FACE('',(#1001),#88,.T.);
#6333=ADVANCED_FACE('',(#1002),#89,.T.);
#6334=ADVANCED_FACE('',(#1003),#6022,.T.);
#6335=ADVANCED_FACE('',(#1004),#147,.F.);
#6336=ADVANCED_FACE('',(#1005),#90,.T.);
#6337=ADVANCED_FACE('',(#1006),#6023,.T.);
#6338=ADVANCED_FACE('',(#1007),#148,.F.);
#6339=ADVANCED_FACE('',(#1008),#149,.F.);
#6340=ADVANCED_FACE('',(#1009),#150,.F.);
#6341=ADVANCED_FACE('',(#1010),#151,.F.);
#6342=ADVANCED_FACE('',(#1011),#152,.F.);
#6343=ADVANCED_FACE('',(#1012),#153,.F.);
#6344=ADVANCED_FACE('',(#1013),#747,.F.);
#6345=ADVANCED_FACE('',(#1014,#614,#615,#616,#617,#618,#619),#748,.T.);
#6346=ADVANCED_FACE('',(#1015),#154,.F.);
#6347=ADVANCED_FACE('',(#1016),#749,.F.);
#6348=ADVANCED_FACE('',(#1017),#6024,.F.);
#6349=ADVANCED_FACE('',(#1018),#6025,.F.);
#6350=ADVANCED_FACE('',(#1019,#620),#750,.T.);
#6351=ADVANCED_FACE('',(#1020),#6026,.T.);
#6352=ADVANCED_FACE('',(#1021),#751,.F.);
#6353=ADVANCED_FACE('',(#1022,#621),#752,.T.);
#6354=ADVANCED_FACE('',(#1023),#6027,.T.);
#6355=ADVANCED_FACE('',(#1024),#753,.F.);
#6356=ADVANCED_FACE('',(#1025,#622),#754,.T.);
#6357=ADVANCED_FACE('',(#1026),#6028,.T.);
#6358=ADVANCED_FACE('',(#1027),#755,.F.);
#6359=ADVANCED_FACE('',(#1028,#623),#756,.T.);
#6360=ADVANCED_FACE('',(#1029),#6029,.T.);
#6361=ADVANCED_FACE('',(#1030),#757,.F.);
#6362=ADVANCED_FACE('',(#1031),#6030,.T.);
#6363=ADVANCED_FACE('',(#1032),#6031,.T.);
#6364=ADVANCED_FACE('',(#1033),#6032,.T.);
#6365=ADVANCED_FACE('',(#1034),#6033,.T.);
#6366=ADVANCED_FACE('',(#1035),#155,.F.);
#6367=ADVANCED_FACE('',(#1036),#6034,.T.);
#6368=ADVANCED_FACE('',(#1037),#156,.F.);
#6369=ADVANCED_FACE('',(#1038),#157,.F.);
#6370=ADVANCED_FACE('',(#1039),#158,.F.);
#6371=ADVANCED_FACE('',(#1040),#6035,.T.);
#6372=ADVANCED_FACE('',(#1041),#159,.F.);
#6373=ADVANCED_FACE('',(#1042),#160,.F.);
#6374=ADVANCED_FACE('',(#1043),#758,.F.);
#6375=ADVANCED_FACE('',(#1044),#161,.F.);
#6376=ADVANCED_FACE('',(#1045),#162,.F.);
#6377=ADVANCED_FACE('',(#1046),#163,.F.);
#6378=ADVANCED_FACE('',(#1047,#624,#625),#759,.T.);
#6379=ADVANCED_FACE('',(#1048),#760,.F.);
#6380=ADVANCED_FACE('',(#1049),#164,.F.);
#6381=ADVANCED_FACE('',(#1050),#165,.F.);
#6382=ADVANCED_FACE('',(#1051,#626,#627,#628,#629,#630,#631),#761,.F.);
#6383=ADVANCED_FACE('',(#1052),#166,.F.);
#6384=ADVANCED_FACE('',(#1053),#6036,.T.);
#6385=ADVANCED_FACE('',(#1054),#6037,.T.);
#6386=ADVANCED_FACE('',(#1055),#6038,.T.);
#6387=ADVANCED_FACE('',(#1056),#6039,.T.);
#6388=ADVANCED_FACE('',(#1057),#6040,.T.);
#6389=ADVANCED_FACE('',(#1058),#6041,.T.);
#6390=ADVANCED_FACE('',(#1059),#6042,.T.);
#6391=ADVANCED_FACE('',(#1060),#6043,.T.);
#6392=ADVANCED_FACE('',(#1061),#6044,.T.);
#6393=ADVANCED_FACE('',(#1062),#6045,.T.);
#6394=ADVANCED_FACE('',(#1063),#6046,.T.);
#6395=ADVANCED_FACE('',(#1064),#6047,.T.);
#6396=ADVANCED_FACE('',(#1065),#6048,.T.);
#6397=ADVANCED_FACE('',(#1066),#6049,.T.);
#6398=ADVANCED_FACE('',(#1067),#6050,.T.);
#6399=ADVANCED_FACE('',(#1068),#6051,.T.);
#6400=ADVANCED_FACE('',(#1069),#6052,.T.);
#6401=ADVANCED_FACE('',(#1070),#6053,.T.);
#6402=ADVANCED_FACE('',(#1071),#6054,.T.);
#6403=ADVANCED_FACE('',(#1072),#6055,.T.);
#6404=ADVANCED_FACE('',(#1073),#6056,.T.);
#6405=ADVANCED_FACE('',(#1074),#6057,.T.);
#6406=ADVANCED_FACE('',(#1075),#6058,.T.);
#6407=ADVANCED_FACE('',(#1076),#6059,.T.);
#6408=ADVANCED_FACE('',(#1077),#6060,.T.);
#6409=ADVANCED_FACE('',(#1078),#6061,.T.);
#6410=ADVANCED_FACE('',(#1079),#6062,.T.);
#6411=ADVANCED_FACE('',(#1080),#6063,.T.);
#6412=ADVANCED_FACE('',(#1081),#6064,.T.);
#6413=ADVANCED_FACE('',(#1082),#6065,.T.);
#6414=ADVANCED_FACE('',(#1083),#6066,.T.);
#6415=ADVANCED_FACE('',(#1084),#6067,.T.);
#6416=ADVANCED_FACE('',(#1085),#6068,.T.);
#6417=ADVANCED_FACE('',(#1086),#6069,.T.);
#6418=ADVANCED_FACE('',(#1087),#6070,.T.);
#6419=ADVANCED_FACE('',(#1088),#6071,.T.);
#6420=ADVANCED_FACE('',(#1089),#6072,.T.);
#6421=ADVANCED_FACE('',(#1090),#6073,.T.);
#6422=ADVANCED_FACE('',(#1091),#6074,.T.);
#6423=ADVANCED_FACE('',(#1092),#6075,.T.);
#6424=ADVANCED_FACE('',(#1093),#6076,.T.);
#6425=ADVANCED_FACE('',(#1094),#6077,.T.);
#6426=ADVANCED_FACE('',(#1095),#6078,.T.);
#6427=ADVANCED_FACE('',(#1096),#6079,.T.);
#6428=ADVANCED_FACE('',(#1097),#6080,.T.);
#6429=ADVANCED_FACE('',(#1098),#6081,.T.);
#6430=ADVANCED_FACE('',(#1099),#6082,.T.);
#6431=ADVANCED_FACE('',(#1100),#6083,.T.);
#6432=ADVANCED_FACE('',(#1101),#6084,.T.);
#6433=ADVANCED_FACE('',(#1102),#6085,.T.);
#6434=ADVANCED_FACE('',(#1103),#6086,.T.);
#6435=ADVANCED_FACE('',(#1104),#6087,.T.);
#6436=ADVANCED_FACE('',(#1105),#6088,.T.);
#6437=ADVANCED_FACE('',(#1106),#6089,.T.);
#6438=ADVANCED_FACE('',(#1107),#6090,.T.);
#6439=ADVANCED_FACE('',(#1108),#6091,.T.);
#6440=ADVANCED_FACE('',(#1109),#6092,.T.);
#6441=ADVANCED_FACE('',(#1110),#6093,.T.);
#6442=ADVANCED_FACE('',(#1111),#6094,.T.);
#6443=ADVANCED_FACE('',(#1112),#6095,.T.);
#6444=ADVANCED_FACE('',(#1113),#639,.T.);
#6445=ADVANCED_FACE('',(#1114),#167,.F.);
#6446=ADVANCED_FACE('',(#1115),#6096,.T.);
#6447=ADVANCED_FACE('',(#1116),#168,.F.);
#6448=ADVANCED_FACE('',(#1117),#6097,.T.);
#6449=ADVANCED_FACE('',(#1118),#762,.F.);
#6450=ADVANCED_FACE('',(#1119),#763,.F.);
#6451=ADVANCED_FACE('',(#1120),#764,.F.);
#6452=ADVANCED_FACE('',(#1121),#765,.F.);
#6453=ADVANCED_FACE('',(#1122),#766,.F.);
#6454=ADVANCED_FACE('',(#1123),#767,.F.);
#6455=ADVANCED_FACE('',(#1124),#768,.F.);
#6456=ADVANCED_FACE('',(#1125,#632),#769,.T.);
#6457=ADVANCED_FACE('',(#1126),#6098,.T.);
#6458=ADVANCED_FACE('',(#1127,#633),#770,.F.);
#6459=ADVANCED_FACE('',(#1128),#771,.T.);
#6460=ADVANCED_FACE('',(#1129),#6099,.F.);
#6461=ADVANCED_FACE('',(#1130),#6100,.F.);
#6462=ADVANCED_FACE('',(#1131),#6101,.F.);
#6463=ADVANCED_FACE('',(#1132),#6102,.F.);
#6464=ADVANCED_FACE('',(#1133),#6103,.F.);
#6465=ADVANCED_FACE('',(#1134),#6104,.F.);
#6466=ADVANCED_FACE('',(#1135),#6105,.F.);
#6467=ADVANCED_FACE('',(#1136),#6106,.F.);
#6468=ADVANCED_FACE('',(#1137),#6107,.F.);
#6469=ADVANCED_FACE('',(#1138),#6108,.F.);
#6470=ADVANCED_FACE('',(#1139),#6109,.F.);
#6471=ADVANCED_FACE('',(#1140),#169,.F.);
#6472=ADVANCED_FACE('',(#1141),#170,.F.);
#6473=ADVANCED_FACE('',(#1142,#634),#772,.T.);
#6474=ADVANCED_FACE('',(#1143),#6110,.F.);
#6475=ADVANCED_FACE('',(#1144),#773,.T.);
#6476=ADVANCED_FACE('',(#1145),#774,.T.);
#6477=ADVANCED_FACE('',(#1146),#775,.T.);
#6478=ADVANCED_FACE('',(#1147),#776,.T.);
#6479=ADVANCED_FACE('',(#1148),#777,.T.);
#6480=ADVANCED_FACE('',(#1149),#778,.T.);
#6481=ADVANCED_FACE('',(#1150,#635),#779,.F.);
#6482=ADVANCED_FACE('',(#1151),#6111,.F.);
#6483=ADVANCED_FACE('',(#1152),#6112,.T.);
#6484=ADVANCED_FACE('',(#1153,#636),#780,.T.);
#6485=ADVANCED_FACE('',(#1154,#637),#781,.F.);
#6486=CLOSED_SHELL('',(#6113,#6114,#6115,#6116,#6117,#6118,#6119,#6120,
#6121,#6122,#6123,#6124,#6125,#6126,#6127,#6128,#6129,#6130,#6131,#6132,
#6133,#6134,#6135,#6136,#6137,#6138,#6139,#6140,#6141,#6142,#6143,#6144));
#6487=CLOSED_SHELL('',(#6145,#6146,#6147,#6148,#6149,#6150,#6151,#6152,
#6153));
#6488=CLOSED_SHELL('',(#6154,#6155,#6156,#6157,#6158,#6159));
#6489=CLOSED_SHELL('',(#6160,#6161,#6162,#6163,#6164,#6165,#6166,#6167,
#6168,#6169,#6170,#6171,#6172,#6173,#6174,#6175,#6176,#6177,#6178,#6179,
#6180,#6181,#6182,#6183,#6184,#6185,#6186,#6187,#6188,#6189,#6190,#6191,
#6192,#6193,#6194,#6195,#6196,#6197,#6198,#6199,#6200,#6201,#6202,#6203,
#6204,#6205,#6206,#6207,#6208,#6209,#6210,#6211,#6212,#6213,#6214,#6215,
#6216,#6217,#6218,#6219,#6220,#6221,#6222,#6223,#6224,#6225,#6226,#6227,
#6228,#6229,#6230,#6231,#6232,#6233,#6234,#6235,#6236,#6237,#6238,#6239,
#6240,#6241,#6242,#6243,#6244,#6245,#6246,#6247,#6248));
#6490=CLOSED_SHELL('',(#6249,#6250,#6251,#6252,#6253,#6254,#6255,#6256,
#6257,#6258,#6259,#6260,#6261,#6262,#6263,#6264,#6265,#6266,#6267,#6268,
#6269,#6270,#6271,#6272,#6273,#6274,#6275,#6276,#6277,#6278,#6279,#6280,
#6281,#6282,#6283,#6284,#6285,#6286,#6287,#6288,#6289,#6290,#6291,#6292,
#6293,#6294,#6295,#6296,#6297,#6298,#6299,#6300,#6301,#6302,#6303,#6304,
#6305,#6306,#6307,#6308,#6309,#6310,#6311,#6312,#6313,#6314,#6315,#6316,
#6317,#6318,#6319,#6320,#6321,#6322,#6323,#6324,#6325,#6326,#6327,#6328,
#6329,#6330,#6331,#6332,#6333,#6334,#6335,#6336,#6337,#6338,#6339,#6340,
#6341,#6342,#6343,#6344,#6345,#6346,#6347));
#6491=CLOSED_SHELL('',(#6348,#6349,#6350,#6351,#6352,#6353,#6354,#6355,
#6356,#6357,#6358,#6359,#6360,#6361,#6362,#6363,#6364,#6365,#6366,#6367,
#6368,#6369,#6370,#6371,#6372,#6373,#6374,#6375,#6376,#6377,#6378,#6379,
#6380,#6381,#6382,#6383));
#6492=CLOSED_SHELL('',(#6384,#6385,#6386,#6387,#6388,#6389,#6390,#6391,
#6392,#6393,#6394,#6395,#6396,#6397,#6398,#6399,#6400,#6401,#6402,#6403,
#6404,#6405,#6406,#6407,#6408,#6409,#6410,#6411,#6412,#6413,#6414,#6415,
#6416,#6417,#6418,#6419,#6420,#6421,#6422,#6423,#6424,#6425,#6426,#6427,
#6428,#6429,#6430,#6431,#6432,#6433,#6434,#6435,#6436,#6437,#6438,#6439,
#6440,#6441,#6442,#6443,#6444,#6445,#6446,#6447,#6448,#6449,#6450,#6451,
#6452,#6453,#6454,#6455,#6456,#6457,#6458,#6459));
#6493=CLOSED_SHELL('',(#6460,#6461,#6462,#6463,#6464,#6465,#6466,#6467,
#6468,#6469,#6470,#6471,#6472,#6473,#6474,#6475,#6476,#6477,#6478,#6479,
#6480,#6481));
#6494=CLOSED_SHELL('',(#6482,#6483,#6484,#6485));
#6495=DERIVED_UNIT_ELEMENT(#6513,1.);
#6496=DERIVED_UNIT_ELEMENT(#18355,-3.);
#6497=DERIVED_UNIT_ELEMENT(#6513,1.);
#6498=DERIVED_UNIT_ELEMENT(#18355,-3.);
#6499=DERIVED_UNIT_ELEMENT(#6513,1.);
#6500=DERIVED_UNIT_ELEMENT(#18355,-3.);
#6501=DERIVED_UNIT_ELEMENT(#6513,1.);
#6502=DERIVED_UNIT_ELEMENT(#18355,-3.);
#6503=DERIVED_UNIT_ELEMENT(#6513,1.);
#6504=DERIVED_UNIT_ELEMENT(#18355,-3.);
#6505=DERIVED_UNIT_ELEMENT(#6513,1.);
#6506=DERIVED_UNIT_ELEMENT(#18355,-3.);
#6507=DERIVED_UNIT_ELEMENT(#6513,1.);
#6508=DERIVED_UNIT_ELEMENT(#18355,-3.);
#6509=DERIVED_UNIT_ELEMENT(#6513,1.);
#6510=DERIVED_UNIT_ELEMENT(#18355,-3.);
#6511=DERIVED_UNIT_ELEMENT(#6513,1.);
#6512=DERIVED_UNIT_ELEMENT(#18355,-3.);
#6513=(
MASS_UNIT()
NAMED_UNIT(*)
SI_UNIT(.KILO.,.GRAM.)
);
#6514=DERIVED_UNIT((#6495,#6496));
#6515=DERIVED_UNIT((#6497,#6498));
#6516=DERIVED_UNIT((#6499,#6500));
#6517=DERIVED_UNIT((#6501,#6502));
#6518=DERIVED_UNIT((#6503,#6504));
#6519=DERIVED_UNIT((#6505,#6506));
#6520=DERIVED_UNIT((#6507,#6508));
#6521=DERIVED_UNIT((#6509,#6510));
#6522=DERIVED_UNIT((#6511,#6512));
#6523=MEASURE_REPRESENTATION_ITEM('density measure',
POSITIVE_RATIO_MEASURE(7850.),#6514);
#6524=MEASURE_REPRESENTATION_ITEM('density measure',
POSITIVE_RATIO_MEASURE(7850.),#6515);
#6525=MEASURE_REPRESENTATION_ITEM('density measure',
POSITIVE_RATIO_MEASURE(7850.),#6516);
#6526=MEASURE_REPRESENTATION_ITEM('density measure',
POSITIVE_RATIO_MEASURE(7850.),#6517);
#6527=MEASURE_REPRESENTATION_ITEM('density measure',
POSITIVE_RATIO_MEASURE(7850.),#6518);
#6528=MEASURE_REPRESENTATION_ITEM('density measure',
POSITIVE_RATIO_MEASURE(7850.),#6519);
#6529=MEASURE_REPRESENTATION_ITEM('density measure',
POSITIVE_RATIO_MEASURE(7850.),#6520);
#6530=MEASURE_REPRESENTATION_ITEM('density measure',
POSITIVE_RATIO_MEASURE(7850.),#6521);
#6531=MEASURE_REPRESENTATION_ITEM('density measure',
POSITIVE_RATIO_MEASURE(7850.),#6522);
#6532=PROPERTY_DEFINITION_REPRESENTATION(#6577,#6550);
#6533=PROPERTY_DEFINITION_REPRESENTATION(#6578,#6551);
#6534=PROPERTY_DEFINITION_REPRESENTATION(#6579,#6552);
#6535=PROPERTY_DEFINITION_REPRESENTATION(#6580,#6553);
#6536=PROPERTY_DEFINITION_REPRESENTATION(#6581,#6554);
#6537=PROPERTY_DEFINITION_REPRESENTATION(#6582,#6555);
#6538=PROPERTY_DEFINITION_REPRESENTATION(#6583,#6556);
#6539=PROPERTY_DEFINITION_REPRESENTATION(#6584,#6557);
#6540=PROPERTY_DEFINITION_REPRESENTATION(#6585,#6558);
#6541=PROPERTY_DEFINITION_REPRESENTATION(#6586,#6559);
#6542=PROPERTY_DEFINITION_REPRESENTATION(#6587,#6560);
#6543=PROPERTY_DEFINITION_REPRESENTATION(#6588,#6561);
#6544=PROPERTY_DEFINITION_REPRESENTATION(#6589,#6562);
#6545=PROPERTY_DEFINITION_REPRESENTATION(#6590,#6563);
#6546=PROPERTY_DEFINITION_REPRESENTATION(#6591,#6564);
#6547=PROPERTY_DEFINITION_REPRESENTATION(#6592,#6565);
#6548=PROPERTY_DEFINITION_REPRESENTATION(#6593,#6566);
#6549=PROPERTY_DEFINITION_REPRESENTATION(#6594,#6567);
#6550=REPRESENTATION('material name',(#6568),#18343);
#6551=REPRESENTATION('density',(#6523),#18343);
#6552=REPRESENTATION('material name',(#6569),#18344);
#6553=REPRESENTATION('density',(#6524),#18344);
#6554=REPRESENTATION('material name',(#6570),#18345);
#6555=REPRESENTATION('density',(#6525),#18345);
#6556=REPRESENTATION('material name',(#6571),#18347);
#6557=REPRESENTATION('density',(#6526),#18347);
#6558=REPRESENTATION('material name',(#6572),#18348);
#6559=REPRESENTATION('density',(#6527),#18348);
#6560=REPRESENTATION('material name',(#6573),#18349);
#6561=REPRESENTATION('density',(#6528),#18349);
#6562=REPRESENTATION('material name',(#6574),#18350);
#6563=REPRESENTATION('density',(#6529),#18350);
#6564=REPRESENTATION('material name',(#6575),#18351);
#6565=REPRESENTATION('density',(#6530),#18351);
#6566=REPRESENTATION('material name',(#6576),#18352);
#6567=REPRESENTATION('density',(#6531),#18352);
#6568=DESCRIPTIVE_REPRESENTATION_ITEM('Steel','Steel');
#6569=DESCRIPTIVE_REPRESENTATION_ITEM('Steel','Steel');
#6570=DESCRIPTIVE_REPRESENTATION_ITEM('Steel','Steel');
#6571=DESCRIPTIVE_REPRESENTATION_ITEM('Steel','Steel');
#6572=DESCRIPTIVE_REPRESENTATION_ITEM('Steel','Steel');
#6573=DESCRIPTIVE_REPRESENTATION_ITEM('Steel','Steel');
#6574=DESCRIPTIVE_REPRESENTATION_ITEM('Steel','Steel');
#6575=DESCRIPTIVE_REPRESENTATION_ITEM('Steel','Steel');
#6576=DESCRIPTIVE_REPRESENTATION_ITEM('Steel','Steel');
#6577=PROPERTY_DEFINITION('material property','material name',#18409);
#6578=PROPERTY_DEFINITION('material property','density of part',#18409);
#6579=PROPERTY_DEFINITION('material property','material name',#18410);
#6580=PROPERTY_DEFINITION('material property','density of part',#18410);
#6581=PROPERTY_DEFINITION('material property','material name',#18411);
#6582=PROPERTY_DEFINITION('material property','density of part',#18411);
#6583=PROPERTY_DEFINITION('material property','material name',#18413);
#6584=PROPERTY_DEFINITION('material property','density of part',#18413);
#6585=PROPERTY_DEFINITION('material property','material name',#18414);
#6586=PROPERTY_DEFINITION('material property','density of part',#18414);
#6587=PROPERTY_DEFINITION('material property','material name',#18415);
#6588=PROPERTY_DEFINITION('material property','density of part',#18415);
#6589=PROPERTY_DEFINITION('material property','material name',#18416);
#6590=PROPERTY_DEFINITION('material property','density of part',#18416);
#6591=PROPERTY_DEFINITION('material property','material name',#18417);
#6592=PROPERTY_DEFINITION('material property','density of part',#18417);
#6593=PROPERTY_DEFINITION('material property','material name',#18418);
#6594=PROPERTY_DEFINITION('material property','density of part',#18418);
#6595=AXIS2_PLACEMENT_3D('',#8460,#7082,#7083);
#6596=AXIS2_PLACEMENT_3D('',#8461,#7084,#7085);
#6597=AXIS2_PLACEMENT_3D('',#8462,#7086,#7087);
#6598=AXIS2_PLACEMENT_3D('',#8464,#7088,#7089);
#6599=AXIS2_PLACEMENT_3D('',#8467,#7091,#7092);
#6600=AXIS2_PLACEMENT_3D('',#8468,#7093,#7094);
#6601=AXIS2_PLACEMENT_3D('',#8470,#7095,#7096);
#6602=AXIS2_PLACEMENT_3D('',#8473,#7098,#7099);
#6603=AXIS2_PLACEMENT_3D('',#8474,#7100,#7101);
#6604=AXIS2_PLACEMENT_3D('',#8476,#7102,#7103);
#6605=AXIS2_PLACEMENT_3D('',#8479,#7105,#7106);
#6606=AXIS2_PLACEMENT_3D('',#8480,#7107,#7108);
#6607=AXIS2_PLACEMENT_3D('',#8487,#7112,#7113);
#6608=AXIS2_PLACEMENT_3D('',#8491,#7115,#7116);
#6609=AXIS2_PLACEMENT_3D('',#8492,#7117,#7118);
#6610=AXIS2_PLACEMENT_3D('',#8493,#7119,#7120);
#6611=AXIS2_PLACEMENT_3D('',#8497,#7123,#7124);
#6612=AXIS2_PLACEMENT_3D('',#8503,#7128,#7129);
#6613=AXIS2_PLACEMENT_3D('',#8512,#7134,#7135);
#6614=AXIS2_PLACEMENT_3D('',#8514,#7136,#7137);
#6615=AXIS2_PLACEMENT_3D('',#8516,#7138,#7139);
#6616=AXIS2_PLACEMENT_3D('',#8518,#7141,#7142);
#6617=AXIS2_PLACEMENT_3D('',#8519,#7143,#7144);
#6618=AXIS2_PLACEMENT_3D('',#8520,#7145,#7146);
#6619=AXIS2_PLACEMENT_3D('',#8521,#7147,#7148);
#6620=AXIS2_PLACEMENT_3D('',#8525,#7151,#7152);
#6621=AXIS2_PLACEMENT_3D('',#8533,#7157,#7158);
#6622=AXIS2_PLACEMENT_3D('',#8539,#7162,#7163);
#6623=AXIS2_PLACEMENT_3D('',#8545,#7167,#7168);
#6624=AXIS2_PLACEMENT_3D('',#8551,#7172,#7173);
#6625=AXIS2_PLACEMENT_3D('',#8553,#7174,#7175);
#6626=AXIS2_PLACEMENT_3D('',#8556,#7177,#7178);
#6627=AXIS2_PLACEMENT_3D('',#8557,#7179,#7180);
#6628=AXIS2_PLACEMENT_3D('',#8559,#7181,#7182);
#6629=AXIS2_PLACEMENT_3D('',#8562,#7184,#7185);
#6630=AXIS2_PLACEMENT_3D('',#8563,#7186,#7187);
#6631=AXIS2_PLACEMENT_3D('',#8567,#7189,#7190);
#6632=AXIS2_PLACEMENT_3D('',#8579,#7196,#7197);
#6633=AXIS2_PLACEMENT_3D('',#8584,#7200,#7201);
#6634=AXIS2_PLACEMENT_3D('',#8585,#7202,#7203);
#6635=AXIS2_PLACEMENT_3D('',#8587,#7204,#7205);
#6636=AXIS2_PLACEMENT_3D('',#8589,#7206,#7207);
#6637=AXIS2_PLACEMENT_3D('',#8590,#7208,#7209);
#6638=AXIS2_PLACEMENT_3D('',#8591,#7210,#7211);
#6639=AXIS2_PLACEMENT_3D('',#8594,#7212,#7213);
#6640=AXIS2_PLACEMENT_3D('',#8595,#7214,#7215);
#6641=AXIS2_PLACEMENT_3D('',#8597,#7217,#7218);
#6642=AXIS2_PLACEMENT_3D('',#8603,#7221,#7222);
#6643=AXIS2_PLACEMENT_3D('',#8615,#7228,#7229);
#6644=AXIS2_PLACEMENT_3D('',#8617,#7231,#7232);
#6645=AXIS2_PLACEMENT_3D('',#8618,#7233,#7234);
#6646=AXIS2_PLACEMENT_3D('',#8619,#7235,#7236);
#6647=AXIS2_PLACEMENT_3D('',#8622,#7239,#7240);
#6648=AXIS2_PLACEMENT_3D('',#8625,#7243,#7244);
#6649=AXIS2_PLACEMENT_3D('',#8627,#7246,#7247);
#6650=AXIS2_PLACEMENT_3D('',#8629,#7249,#7250);
#6651=AXIS2_PLACEMENT_3D('',#8630,#7251,#7252);
#6652=AXIS2_PLACEMENT_3D('',#8632,#7254,#7255);
#6653=AXIS2_PLACEMENT_3D('',#8633,#7256,#7257);
#6654=AXIS2_PLACEMENT_3D('',#8635,#7259,#7260);
#6655=AXIS2_PLACEMENT_3D('',#8637,#7262,#7263);
#6656=AXIS2_PLACEMENT_3D('',#8638,#7264,#7265);
#6657=AXIS2_PLACEMENT_3D('',#8639,#7266,#7267);
#6658=AXIS2_PLACEMENT_3D('',#8641,#7268,#7269);
#6659=AXIS2_PLACEMENT_3D('',#8644,#7271,#7272);
#6660=AXIS2_PLACEMENT_3D('',#8645,#7273,#7274);
#6661=AXIS2_PLACEMENT_3D('',#8647,#7275,#7276);
#6662=AXIS2_PLACEMENT_3D('',#8648,#7277,#7278);
#6663=AXIS2_PLACEMENT_3D('',#8650,#7279,#7280);
#6664=AXIS2_PLACEMENT_3D('',#8651,#7281,#7282);
#6665=AXIS2_PLACEMENT_3D('',#8653,#7283,#7284);
#6666=AXIS2_PLACEMENT_3D('',#8655,#7286,#7287);
#6667=AXIS2_PLACEMENT_3D('',#8657,#7288,#7289);
#6668=AXIS2_PLACEMENT_3D('',#8659,#7290,#7291);
#6669=AXIS2_PLACEMENT_3D('',#8660,#7292,#7293);
#6670=AXIS2_PLACEMENT_3D('',#8663,#7295,#7296);
#6671=AXIS2_PLACEMENT_3D('',#8664,#7297,#7298);
#6672=AXIS2_PLACEMENT_3D('',#8665,#7299,#7300);
#6673=AXIS2_PLACEMENT_3D('',#8667,#7302,#7303);
#6674=AXIS2_PLACEMENT_3D('',#8668,#7304,#7305);
#6675=AXIS2_PLACEMENT_3D('',#8669,#7306,#7307);
#6676=AXIS2_PLACEMENT_3D('',#8678,#7312,#7313);
#6677=AXIS2_PLACEMENT_3D('',#8687,#7318,#7319);
#6678=AXIS2_PLACEMENT_3D('',#8688,#7320,#7321);
#6679=AXIS2_PLACEMENT_3D('',#8689,#7322,#7323);
#6680=AXIS2_PLACEMENT_3D('',#8690,#7324,#7325);
#6681=AXIS2_PLACEMENT_3D('',#8691,#7326,#7327);
#6682=AXIS2_PLACEMENT_3D('',#8692,#7328,#7329);
#6683=AXIS2_PLACEMENT_3D('',#8693,#7330,#7331);
#6684=AXIS2_PLACEMENT_3D('',#8694,#7332,#7333);
#6685=AXIS2_PLACEMENT_3D('',#8695,#7334,#7335);
#6686=AXIS2_PLACEMENT_3D('',#8696,#7336,#7337);
#6687=AXIS2_PLACEMENT_3D('',#8697,#7338,#7339);
#6688=AXIS2_PLACEMENT_3D('',#8699,#7340,#7341);
#6689=AXIS2_PLACEMENT_3D('',#8702,#7343,#7344);
#6690=AXIS2_PLACEMENT_3D('',#8703,#7345,#7346);
#6691=AXIS2_PLACEMENT_3D('',#8705,#7347,#7348);
#6692=AXIS2_PLACEMENT_3D('',#8708,#7350,#7351);
#6693=AXIS2_PLACEMENT_3D('',#8709,#7352,#7353);
#6694=AXIS2_PLACEMENT_3D('',#8711,#7354,#7355);
#6695=AXIS2_PLACEMENT_3D('',#8714,#7357,#7358);
#6696=AXIS2_PLACEMENT_3D('',#8715,#7359,#7360);
#6697=AXIS2_PLACEMENT_3D('',#8717,#7361,#7362);
#6698=AXIS2_PLACEMENT_3D('',#8720,#7364,#7365);
#6699=AXIS2_PLACEMENT_3D('',#8721,#7366,#7367);
#6700=AXIS2_PLACEMENT_3D('',#8723,#7368,#7369);
#6701=AXIS2_PLACEMENT_3D('',#8726,#7371,#7372);
#6702=AXIS2_PLACEMENT_3D('',#8727,#7373,#7374);
#6703=AXIS2_PLACEMENT_3D('',#8729,#7375,#7376);
#6704=AXIS2_PLACEMENT_3D('',#8730,#7377,#7378);
#6705=AXIS2_PLACEMENT_3D('',#8732,#7379,#7380);
#6706=AXIS2_PLACEMENT_3D('',#8735,#7382,#7383);
#6707=AXIS2_PLACEMENT_3D('',#8736,#7384,#7385);
#6708=AXIS2_PLACEMENT_3D('',#8738,#7386,#7387);
#6709=AXIS2_PLACEMENT_3D('',#8739,#7388,#7389);
#6710=AXIS2_PLACEMENT_3D('',#8742,#7391,#7392);
#6711=AXIS2_PLACEMENT_3D('',#8743,#7393,#7394);
#6712=AXIS2_PLACEMENT_3D('',#8746,#7396,#7397);
#6713=AXIS2_PLACEMENT_3D('',#8747,#7398,#7399);
#6714=AXIS2_PLACEMENT_3D('',#8756,#7404,#7405);
#6715=AXIS2_PLACEMENT_3D('',#8765,#7410,#7411);
#6716=AXIS2_PLACEMENT_3D('',#8774,#7416,#7417);
#6717=AXIS2_PLACEMENT_3D('',#8783,#7422,#7423);
#6718=AXIS2_PLACEMENT_3D('',#8792,#7428,#7429);
#6719=AXIS2_PLACEMENT_3D('',#8801,#7434,#7435);
#6720=AXIS2_PLACEMENT_3D('',#8810,#7440,#7441);
#6721=AXIS2_PLACEMENT_3D('',#8812,#7442,#7443);
#6722=AXIS2_PLACEMENT_3D('',#8813,#7444,#7445);
#6723=AXIS2_PLACEMENT_3D('',#8815,#7446,#7447);
#6724=AXIS2_PLACEMENT_3D('',#8816,#7448,#7449);
#6725=AXIS2_PLACEMENT_3D('',#8819,#7452,#7453);
#6726=AXIS2_PLACEMENT_3D('',#8822,#7456,#7457);
#6727=AXIS2_PLACEMENT_3D('',#8825,#7460,#7461);
#6728=AXIS2_PLACEMENT_3D('',#8831,#7465,#7466);
#6729=AXIS2_PLACEMENT_3D('',#8837,#7470,#7471);
#6730=AXIS2_PLACEMENT_3D('',#8914,#7474,#7475);
#6731=AXIS2_PLACEMENT_3D('',#8992,#7479,#7480);
#6732=AXIS2_PLACEMENT_3D('',#9070,#7484,#7485);
#6733=AXIS2_PLACEMENT_3D('',#9148,#7489,#7490);
#6734=AXIS2_PLACEMENT_3D('',#9164,#7494,#7495);
#6735=AXIS2_PLACEMENT_3D('',#9488,#7507,#7508);
#6736=AXIS2_PLACEMENT_3D('',#9490,#7509,#7510);
#6737=AXIS2_PLACEMENT_3D('',#9492,#7512,#7513);
#6738=AXIS2_PLACEMENT_3D('',#9494,#7514,#7515);
#6739=AXIS2_PLACEMENT_3D('',#9496,#7517,#7518);
#6740=AXIS2_PLACEMENT_3D('',#9664,#7520,#7521);
#6741=AXIS2_PLACEMENT_3D('',#9665,#7522,#7523);
#6742=AXIS2_PLACEMENT_3D('',#9670,#7524,#7525);
#6743=AXIS2_PLACEMENT_3D('',#9742,#7527,#7528);
#6744=AXIS2_PLACEMENT_3D('',#9860,#7530,#7531);
#6745=AXIS2_PLACEMENT_3D('',#9905,#7532,#7533);
#6746=AXIS2_PLACEMENT_3D('',#10023,#7535,#7536);
#6747=AXIS2_PLACEMENT_3D('',#10068,#7537,#7538);
#6748=AXIS2_PLACEMENT_3D('',#10188,#7540,#7541);
#6749=AXIS2_PLACEMENT_3D('',#10193,#7542,#7543);
#6750=AXIS2_PLACEMENT_3D('',#10245,#7545,#7546);
#6751=AXIS2_PLACEMENT_3D('',#10246,#7547,#7548);
#6752=AXIS2_PLACEMENT_3D('',#10247,#7549,#7550);
#6753=AXIS2_PLACEMENT_3D('',#10248,#7551,#7552);
#6754=AXIS2_PLACEMENT_3D('',#10249,#7553,#7554);
#6755=AXIS2_PLACEMENT_3D('',#10250,#7555,#7556);
#6756=AXIS2_PLACEMENT_3D('',#10252,#7557,#7558);
#6757=AXIS2_PLACEMENT_3D('',#10253,#7559,#7560);
#6758=AXIS2_PLACEMENT_3D('',#10254,#7561,#7562);
#6759=AXIS2_PLACEMENT_3D('',#10255,#7563,#7564);
#6760=AXIS2_PLACEMENT_3D('',#10256,#7565,#7566);
#6761=AXIS2_PLACEMENT_3D('',#10257,#7567,#7568);
#6762=AXIS2_PLACEMENT_3D('',#10278,#7569,#7570);
#6763=AXIS2_PLACEMENT_3D('',#10280,#7571,#7572);
#6764=AXIS2_PLACEMENT_3D('',#10281,#7573,#7574);
#6765=AXIS2_PLACEMENT_3D('',#10282,#7575,#7576);
#6766=AXIS2_PLACEMENT_3D('',#10372,#7578,#7579);
#6767=AXIS2_PLACEMENT_3D('',#10373,#7580,#7581);
#6768=AXIS2_PLACEMENT_3D('',#10376,#7582,#7583);
#6769=AXIS2_PLACEMENT_3D('',#10378,#7584,#7585);
#6770=AXIS2_PLACEMENT_3D('',#10379,#7586,#7587);
#6771=AXIS2_PLACEMENT_3D('',#10380,#7588,#7589);
#6772=AXIS2_PLACEMENT_3D('',#10383,#7590,#7591);
#6773=AXIS2_PLACEMENT_3D('',#10385,#7592,#7593);
#6774=AXIS2_PLACEMENT_3D('',#10386,#7594,#7595);
#6775=AXIS2_PLACEMENT_3D('',#10387,#7596,#7597);
#6776=AXIS2_PLACEMENT_3D('',#10390,#7598,#7599);
#6777=AXIS2_PLACEMENT_3D('',#10392,#7600,#7601);
#6778=AXIS2_PLACEMENT_3D('',#10393,#7602,#7603);
#6779=AXIS2_PLACEMENT_3D('',#10394,#7604,#7605);
#6780=AXIS2_PLACEMENT_3D('',#10425,#7608,#7609);
#6781=AXIS2_PLACEMENT_3D('',#10428,#7610,#7611);
#6782=AXIS2_PLACEMENT_3D('',#10430,#7612,#7613);
#6783=AXIS2_PLACEMENT_3D('',#10431,#7614,#7615);
#6784=AXIS2_PLACEMENT_3D('',#10432,#7616,#7617);
#6785=AXIS2_PLACEMENT_3D('',#10612,#7620,#7621);
#6786=AXIS2_PLACEMENT_3D('',#10613,#7622,#7623);
#6787=AXIS2_PLACEMENT_3D('',#10630,#7624,#7625);
#6788=AXIS2_PLACEMENT_3D('',#10631,#7626,#7627);
#6789=AXIS2_PLACEMENT_3D('',#10632,#7628,#7629);
#6790=AXIS2_PLACEMENT_3D('',#10634,#7630,#7631);
#6791=AXIS2_PLACEMENT_3D('',#10637,#7633,#7634);
#6792=AXIS2_PLACEMENT_3D('',#10638,#7635,#7636);
#6793=AXIS2_PLACEMENT_3D('',#10640,#7637,#7638);
#6794=AXIS2_PLACEMENT_3D('',#10643,#7640,#7641);
#6795=AXIS2_PLACEMENT_3D('',#10644,#7642,#7643);
#6796=AXIS2_PLACEMENT_3D('',#10646,#7644,#7645);
#6797=AXIS2_PLACEMENT_3D('',#10649,#7647,#7648);
#6798=AXIS2_PLACEMENT_3D('',#10650,#7649,#7650);
#6799=AXIS2_PLACEMENT_3D('',#10652,#7651,#7652);
#6800=AXIS2_PLACEMENT_3D('',#10655,#7654,#7655);
#6801=AXIS2_PLACEMENT_3D('',#10656,#7656,#7657);
#6802=AXIS2_PLACEMENT_3D('',#10665,#7662,#7663);
#6803=AXIS2_PLACEMENT_3D('',#10671,#7667,#7668);
#6804=AXIS2_PLACEMENT_3D('',#10677,#7672,#7673);
#6805=AXIS2_PLACEMENT_3D('',#10683,#7677,#7678);
#6806=AXIS2_PLACEMENT_3D('',#10689,#7682,#7683);
#6807=AXIS2_PLACEMENT_3D('',#10692,#7686,#7687);
#6808=AXIS2_PLACEMENT_3D('',#10694,#7688,#7689);
#6809=AXIS2_PLACEMENT_3D('',#10695,#7690,#7691);
#6810=AXIS2_PLACEMENT_3D('',#10704,#7696,#7697);
#6811=AXIS2_PLACEMENT_3D('',#10710,#7701,#7702);
#6812=AXIS2_PLACEMENT_3D('',#10716,#7706,#7707);
#6813=AXIS2_PLACEMENT_3D('',#10722,#7711,#7712);
#6814=AXIS2_PLACEMENT_3D('',#10728,#7716,#7717);
#6815=AXIS2_PLACEMENT_3D('',#10731,#7720,#7721);
#6816=AXIS2_PLACEMENT_3D('',#10733,#7722,#7723);
#6817=AXIS2_PLACEMENT_3D('',#10734,#7724,#7725);
#6818=AXIS2_PLACEMENT_3D('',#10737,#7727,#7728);
#6819=AXIS2_PLACEMENT_3D('',#10738,#7729,#7730);
#6820=AXIS2_PLACEMENT_3D('',#10741,#7732,#7733);
#6821=AXIS2_PLACEMENT_3D('',#10742,#7734,#7735);
#6822=AXIS2_PLACEMENT_3D('',#10751,#7740,#7741);
#6823=AXIS2_PLACEMENT_3D('',#10760,#7746,#7747);
#6824=AXIS2_PLACEMENT_3D('',#10769,#7752,#7753);
#6825=AXIS2_PLACEMENT_3D('',#10778,#7758,#7759);
#6826=AXIS2_PLACEMENT_3D('',#10787,#7764,#7765);
#6827=AXIS2_PLACEMENT_3D('',#10796,#7770,#7771);
#6828=AXIS2_PLACEMENT_3D('',#10805,#7776,#7777);
#6829=AXIS2_PLACEMENT_3D('',#10807,#7778,#7779);
#6830=AXIS2_PLACEMENT_3D('',#10808,#7780,#7781);
#6831=AXIS2_PLACEMENT_3D('',#10810,#7782,#7783);
#6832=AXIS2_PLACEMENT_3D('',#10811,#7784,#7785);
#6833=AXIS2_PLACEMENT_3D('',#10814,#7788,#7789);
#6834=AXIS2_PLACEMENT_3D('',#10817,#7792,#7793);
#6835=AXIS2_PLACEMENT_3D('',#10820,#7796,#7797);
#6836=AXIS2_PLACEMENT_3D('',#10826,#7801,#7802);
#6837=AXIS2_PLACEMENT_3D('',#10832,#7806,#7807);
#6838=AXIS2_PLACEMENT_3D('',#10909,#7810,#7811);
#6839=AXIS2_PLACEMENT_3D('',#10987,#7815,#7816);
#6840=AXIS2_PLACEMENT_3D('',#11065,#7820,#7821);
#6841=AXIS2_PLACEMENT_3D('',#11143,#7825,#7826);
#6842=AXIS2_PLACEMENT_3D('',#11159,#7830,#7831);
#6843=AXIS2_PLACEMENT_3D('',#11483,#7843,#7844);
#6844=AXIS2_PLACEMENT_3D('',#11485,#7845,#7846);
#6845=AXIS2_PLACEMENT_3D('',#11487,#7848,#7849);
#6846=AXIS2_PLACEMENT_3D('',#11489,#7850,#7851);
#6847=AXIS2_PLACEMENT_3D('',#11491,#7853,#7854);
#6848=AXIS2_PLACEMENT_3D('',#11659,#7856,#7857);
#6849=AXIS2_PLACEMENT_3D('',#11660,#7858,#7859);
#6850=AXIS2_PLACEMENT_3D('',#11665,#7860,#7861);
#6851=AXIS2_PLACEMENT_3D('',#11737,#7863,#7864);
#6852=AXIS2_PLACEMENT_3D('',#11855,#7866,#7867);
#6853=AXIS2_PLACEMENT_3D('',#11900,#7868,#7869);
#6854=AXIS2_PLACEMENT_3D('',#12018,#7871,#7872);
#6855=AXIS2_PLACEMENT_3D('',#12063,#7873,#7874);
#6856=AXIS2_PLACEMENT_3D('',#12183,#7876,#7877);
#6857=AXIS2_PLACEMENT_3D('',#12188,#7878,#7879);
#6858=AXIS2_PLACEMENT_3D('',#12240,#7881,#7882);
#6859=AXIS2_PLACEMENT_3D('',#12241,#7883,#7884);
#6860=AXIS2_PLACEMENT_3D('',#12242,#7885,#7886);
#6861=AXIS2_PLACEMENT_3D('',#12243,#7887,#7888);
#6862=AXIS2_PLACEMENT_3D('',#12244,#7889,#7890);
#6863=AXIS2_PLACEMENT_3D('',#12245,#7891,#7892);
#6864=AXIS2_PLACEMENT_3D('',#12247,#7893,#7894);
#6865=AXIS2_PLACEMENT_3D('',#12248,#7895,#7896);
#6866=AXIS2_PLACEMENT_3D('',#12249,#7897,#7898);
#6867=AXIS2_PLACEMENT_3D('',#12250,#7899,#7900);
#6868=AXIS2_PLACEMENT_3D('',#12251,#7901,#7902);
#6869=AXIS2_PLACEMENT_3D('',#12252,#7903,#7904);
#6870=AXIS2_PLACEMENT_3D('',#12273,#7905,#7906);
#6871=AXIS2_PLACEMENT_3D('',#12275,#7907,#7908);
#6872=AXIS2_PLACEMENT_3D('',#12276,#7909,#7910);
#6873=AXIS2_PLACEMENT_3D('',#12277,#7911,#7912);
#6874=AXIS2_PLACEMENT_3D('',#12367,#7914,#7915);
#6875=AXIS2_PLACEMENT_3D('',#12368,#7916,#7917);
#6876=AXIS2_PLACEMENT_3D('',#12371,#7918,#7919);
#6877=AXIS2_PLACEMENT_3D('',#12373,#7920,#7921);
#6878=AXIS2_PLACEMENT_3D('',#12374,#7922,#7923);
#6879=AXIS2_PLACEMENT_3D('',#12375,#7924,#7925);
#6880=AXIS2_PLACEMENT_3D('',#12378,#7926,#7927);
#6881=AXIS2_PLACEMENT_3D('',#12380,#7928,#7929);
#6882=AXIS2_PLACEMENT_3D('',#12381,#7930,#7931);
#6883=AXIS2_PLACEMENT_3D('',#12382,#7932,#7933);
#6884=AXIS2_PLACEMENT_3D('',#12385,#7934,#7935);
#6885=AXIS2_PLACEMENT_3D('',#12387,#7936,#7937);
#6886=AXIS2_PLACEMENT_3D('',#12388,#7938,#7939);
#6887=AXIS2_PLACEMENT_3D('',#12389,#7940,#7941);
#6888=AXIS2_PLACEMENT_3D('',#12420,#7944,#7945);
#6889=AXIS2_PLACEMENT_3D('',#12423,#7946,#7947);
#6890=AXIS2_PLACEMENT_3D('',#12425,#7948,#7949);
#6891=AXIS2_PLACEMENT_3D('',#12426,#7950,#7951);
#6892=AXIS2_PLACEMENT_3D('',#12427,#7952,#7953);
#6893=AXIS2_PLACEMENT_3D('',#12607,#7956,#7957);
#6894=AXIS2_PLACEMENT_3D('',#12608,#7958,#7959);
#6895=AXIS2_PLACEMENT_3D('',#12625,#7960,#7961);
#6896=AXIS2_PLACEMENT_3D('',#12626,#7962,#7963);
#6897=AXIS2_PLACEMENT_3D('',#12627,#7964,#7965);
#6898=AXIS2_PLACEMENT_3D('',#12629,#7966,#7967);
#6899=AXIS2_PLACEMENT_3D('',#12632,#7969,#7970);
#6900=AXIS2_PLACEMENT_3D('',#12633,#7971,#7972);
#6901=AXIS2_PLACEMENT_3D('',#12635,#7973,#7974);
#6902=AXIS2_PLACEMENT_3D('',#12638,#7976,#7977);
#6903=AXIS2_PLACEMENT_3D('',#12639,#7978,#7979);
#6904=AXIS2_PLACEMENT_3D('',#12641,#7980,#7981);
#6905=AXIS2_PLACEMENT_3D('',#12643,#7982,#7983);
#6906=AXIS2_PLACEMENT_3D('',#12644,#7984,#7985);
#6907=AXIS2_PLACEMENT_3D('',#12646,#7986,#7987);
#6908=AXIS2_PLACEMENT_3D('',#12648,#7989,#7990);
#6909=AXIS2_PLACEMENT_3D('',#12649,#7991,#7992);
#6910=AXIS2_PLACEMENT_3D('',#12651,#7993,#7994);
#6911=AXIS2_PLACEMENT_3D('',#12653,#7995,#7996);
#6912=AXIS2_PLACEMENT_3D('',#12654,#7997,#7998);
#6913=AXIS2_PLACEMENT_3D('',#12656,#7999,#8000);
#6914=AXIS2_PLACEMENT_3D('',#12658,#8002,#8003);
#6915=AXIS2_PLACEMENT_3D('',#12659,#8004,#8005);
#6916=AXIS2_PLACEMENT_3D('',#12661,#8006,#8007);
#6917=AXIS2_PLACEMENT_3D('',#12663,#8008,#8009);
#6918=AXIS2_PLACEMENT_3D('',#12664,#8010,#8011);
#6919=AXIS2_PLACEMENT_3D('',#12666,#8012,#8013);
#6920=AXIS2_PLACEMENT_3D('',#12668,#8015,#8016);
#6921=AXIS2_PLACEMENT_3D('',#12669,#8017,#8018);
#6922=AXIS2_PLACEMENT_3D('',#12671,#8019,#8020);
#6923=AXIS2_PLACEMENT_3D('',#12673,#8021,#8022);
#6924=AXIS2_PLACEMENT_3D('',#12674,#8023,#8024);
#6925=AXIS2_PLACEMENT_3D('',#12676,#8025,#8026);
#6926=AXIS2_PLACEMENT_3D('',#12678,#8028,#8029);
#6927=AXIS2_PLACEMENT_3D('',#12679,#8030,#8031);
#6928=AXIS2_PLACEMENT_3D('',#12682,#8033,#8034);
#6929=AXIS2_PLACEMENT_3D('',#12683,#8035,#8036);
#6930=AXIS2_PLACEMENT_3D('',#12686,#8038,#8039);
#6931=AXIS2_PLACEMENT_3D('',#12687,#8040,#8041);
#6932=AXIS2_PLACEMENT_3D('',#12690,#8043,#8044);
#6933=AXIS2_PLACEMENT_3D('',#12691,#8045,#8046);
#6934=AXIS2_PLACEMENT_3D('',#12694,#8048,#8049);
#6935=AXIS2_PLACEMENT_3D('',#12722,#8050,#8051);
#6936=AXIS2_PLACEMENT_3D('',#12730,#8052,#8053);
#6937=AXIS2_PLACEMENT_3D('',#12736,#8054,#8055);
#6938=AXIS2_PLACEMENT_3D('',#12739,#8056,#8057);
#6939=AXIS2_PLACEMENT_3D('',#12769,#8060,#8061);
#6940=AXIS2_PLACEMENT_3D('',#12812,#8062,#8063);
#6941=AXIS2_PLACEMENT_3D('',#12852,#8064,#8065);
#6942=AXIS2_PLACEMENT_3D('',#12863,#8066,#8067);
#6943=AXIS2_PLACEMENT_3D('',#12866,#8068,#8069);
#6944=AXIS2_PLACEMENT_3D('',#12896,#8072,#8073);
#6945=AXIS2_PLACEMENT_3D('',#12949,#8074,#8075);
#6946=AXIS2_PLACEMENT_3D('',#13089,#8077,#8078);
#6947=AXIS2_PLACEMENT_3D('',#13090,#8079,#8080);
#6948=AXIS2_PLACEMENT_3D('',#13200,#8082,#8083);
#6949=AXIS2_PLACEMENT_3D('',#13221,#8084,#8085);
#6950=AXIS2_PLACEMENT_3D('',#13222,#8086,#8087);
#6951=AXIS2_PLACEMENT_3D('',#13238,#8089,#8090);
#6952=AXIS2_PLACEMENT_3D('',#13246,#8091,#8092);
#6953=AXIS2_PLACEMENT_3D('',#13294,#8094,#8095);
#6954=AXIS2_PLACEMENT_3D('',#13342,#8097,#8098);
#6955=AXIS2_PLACEMENT_3D('',#13393,#8100,#8101);
#6956=AXIS2_PLACEMENT_3D('',#13441,#8103,#8104);
#6957=AXIS2_PLACEMENT_3D('',#13489,#8106,#8107);
#6958=AXIS2_PLACEMENT_3D('',#13537,#8109,#8110);
#6959=AXIS2_PLACEMENT_3D('',#13591,#8112,#8113);
#6960=AXIS2_PLACEMENT_3D('',#13639,#8115,#8116);
#6961=AXIS2_PLACEMENT_3D('',#13687,#8118,#8119);
#6962=AXIS2_PLACEMENT_3D('',#13741,#8121,#8122);
#6963=AXIS2_PLACEMENT_3D('',#13789,#8124,#8125);
#6964=AXIS2_PLACEMENT_3D('',#13837,#8127,#8128);
#6965=AXIS2_PLACEMENT_3D('',#13885,#8130,#8131);
#6966=AXIS2_PLACEMENT_3D('',#13939,#8133,#8134);
#6967=AXIS2_PLACEMENT_3D('',#13987,#8136,#8137);
#6968=AXIS2_PLACEMENT_3D('',#14035,#8139,#8140);
#6969=AXIS2_PLACEMENT_3D('',#14089,#8142,#8143);
#6970=AXIS2_PLACEMENT_3D('',#14137,#8145,#8146);
#6971=AXIS2_PLACEMENT_3D('',#14185,#8148,#8149);
#6972=AXIS2_PLACEMENT_3D('',#14239,#8151,#8152);
#6973=AXIS2_PLACEMENT_3D('',#14287,#8154,#8155);
#6974=AXIS2_PLACEMENT_3D('',#14335,#8157,#8158);
#6975=AXIS2_PLACEMENT_3D('',#14383,#8160,#8161);
#6976=AXIS2_PLACEMENT_3D('',#14437,#8163,#8164);
#6977=AXIS2_PLACEMENT_3D('',#14485,#8166,#8167);
#6978=AXIS2_PLACEMENT_3D('',#14533,#8169,#8170);
#6979=AXIS2_PLACEMENT_3D('',#14587,#8172,#8173);
#6980=AXIS2_PLACEMENT_3D('',#14635,#8175,#8176);
#6981=AXIS2_PLACEMENT_3D('',#14683,#8178,#8179);
#6982=AXIS2_PLACEMENT_3D('',#14699,#8181,#8182);
#6983=AXIS2_PLACEMENT_3D('',#14709,#8183,#8184);
#6984=AXIS2_PLACEMENT_3D('',#14733,#8186,#8187);
#6985=AXIS2_PLACEMENT_3D('',#14757,#8189,#8190);
#6986=AXIS2_PLACEMENT_3D('',#14782,#8192,#8193);
#6987=AXIS2_PLACEMENT_3D('',#14807,#8195,#8196);
#6988=AXIS2_PLACEMENT_3D('',#14831,#8198,#8199);
#6989=AXIS2_PLACEMENT_3D('',#14856,#8201,#8202);
#6990=AXIS2_PLACEMENT_3D('',#14881,#8204,#8205);
#6991=AXIS2_PLACEMENT_3D('',#14905,#8207,#8208);
#6992=AXIS2_PLACEMENT_3D('',#14929,#8210,#8211);
#6993=AXIS2_PLACEMENT_3D('',#14954,#8213,#8214);
#6994=AXIS2_PLACEMENT_3D('',#14979,#8216,#8217);
#6995=AXIS2_PLACEMENT_3D('',#15003,#8219,#8220);
#6996=AXIS2_PLACEMENT_3D('',#15028,#8222,#8223);
#6997=AXIS2_PLACEMENT_3D('',#15053,#8225,#8226);
#6998=AXIS2_PLACEMENT_3D('',#15077,#8228,#8229);
#6999=AXIS2_PLACEMENT_3D('',#15102,#8231,#8232);
#7000=AXIS2_PLACEMENT_3D('',#15127,#8234,#8235);
#7001=AXIS2_PLACEMENT_3D('',#15151,#8237,#8238);
#7002=AXIS2_PLACEMENT_3D('',#15175,#8240,#8241);
#7003=AXIS2_PLACEMENT_3D('',#15200,#8243,#8244);
#7004=AXIS2_PLACEMENT_3D('',#15225,#8246,#8247);
#7005=AXIS2_PLACEMENT_3D('',#15249,#8249,#8250);
#7006=AXIS2_PLACEMENT_3D('',#15274,#8252,#8253);
#7007=AXIS2_PLACEMENT_3D('',#15299,#8255,#8256);
#7008=AXIS2_PLACEMENT_3D('',#15323,#8258,#8259);
#7009=AXIS2_PLACEMENT_3D('',#15348,#8261,#8262);
#7010=AXIS2_PLACEMENT_3D('',#15372,#8264,#8265);
#7011=AXIS2_PLACEMENT_3D('',#15397,#8267,#8268);
#7012=AXIS2_PLACEMENT_3D('',#15421,#8270,#8271);
#7013=AXIS2_PLACEMENT_3D('',#15583,#8272,#8273);
#7014=AXIS2_PLACEMENT_3D('',#15602,#8275,#8276);
#7015=AXIS2_PLACEMENT_3D('',#16464,#8277,#8278);
#7016=AXIS2_PLACEMENT_3D('',#16475,#8279,#8280);
#7017=AXIS2_PLACEMENT_3D('',#17342,#8281,#8282);
#7018=AXIS2_PLACEMENT_3D('',#17343,#8283,#8284);
#7019=AXIS2_PLACEMENT_3D('',#17352,#8289,#8290);
#7020=AXIS2_PLACEMENT_3D('',#17358,#8294,#8295);
#7021=AXIS2_PLACEMENT_3D('',#17364,#8299,#8300);
#7022=AXIS2_PLACEMENT_3D('',#17370,#8304,#8305);
#7023=AXIS2_PLACEMENT_3D('',#17376,#8309,#8310);
#7024=AXIS2_PLACEMENT_3D('',#17379,#8313,#8314);
#7025=AXIS2_PLACEMENT_3D('',#17380,#8315,#8316);
#7026=AXIS2_PLACEMENT_3D('',#17382,#8317,#8318);
#7027=AXIS2_PLACEMENT_3D('',#17383,#8319,#8320);
#7028=AXIS2_PLACEMENT_3D('',#17386,#8322,#8323);
#7029=AXIS2_PLACEMENT_3D('',#17387,#8324,#8325);
#7030=AXIS2_PLACEMENT_3D('',#17388,#8326,#8327);
#7031=AXIS2_PLACEMENT_3D('',#17389,#8328,#8329);
#7032=AXIS2_PLACEMENT_3D('',#17390,#8330,#8331);
#7033=AXIS2_PLACEMENT_3D('',#17395,#8333,#8334);
#7034=AXIS2_PLACEMENT_3D('',#17403,#8335,#8336);
#7035=AXIS2_PLACEMENT_3D('',#17427,#8338,#8339);
#7036=AXIS2_PLACEMENT_3D('',#17450,#8340,#8341);
#7037=AXIS2_PLACEMENT_3D('',#17504,#8343,#8344);
#7038=AXIS2_PLACEMENT_3D('',#17552,#8346,#8347);
#7039=AXIS2_PLACEMENT_3D('',#17571,#8349,#8350);
#7040=AXIS2_PLACEMENT_3D('',#17591,#8351,#8352);
#7041=AXIS2_PLACEMENT_3D('',#17604,#8354,#8355);
#7042=AXIS2_PLACEMENT_3D('',#17612,#8356,#8357);
#7043=AXIS2_PLACEMENT_3D('',#17637,#8359,#8360);
#7044=AXIS2_PLACEMENT_3D('',#17662,#8362,#8363);
#7045=AXIS2_PLACEMENT_3D('',#17687,#8365,#8366);
#7046=AXIS2_PLACEMENT_3D('',#17698,#8368,#8369);
#7047=AXIS2_PLACEMENT_3D('',#17704,#8370,#8371);
#7048=AXIS2_PLACEMENT_3D('',#18260,#8372,#8373);
#7049=AXIS2_PLACEMENT_3D('',#18273,#8380,#8381);
#7050=AXIS2_PLACEMENT_3D('',#18274,#8382,#8383);
#7051=AXIS2_PLACEMENT_3D('',#18280,#8387,#8388);
#7052=AXIS2_PLACEMENT_3D('',#18284,#8391,#8392);
#7053=AXIS2_PLACEMENT_3D('',#18288,#8395,#8396);
#7054=AXIS2_PLACEMENT_3D('',#18292,#8399,#8400);
#7055=AXIS2_PLACEMENT_3D('',#18296,#8403,#8404);
#7056=AXIS2_PLACEMENT_3D('',#18298,#8406,#8407);
#7057=AXIS2_PLACEMENT_3D('',#18299,#8408,#8409);
#7058=AXIS2_PLACEMENT_3D('',#18300,#8410,#8411);
#7059=AXIS2_PLACEMENT_3D('',#18301,#8412,#8413);
#7060=AXIS2_PLACEMENT_3D('',#18302,#8414,#8415);
#7061=AXIS2_PLACEMENT_3D('',#18303,#8416,#8417);
#7062=AXIS2_PLACEMENT_3D('',#18304,#8418,#8419);
#7063=AXIS2_PLACEMENT_3D('',#18305,#8420,#8421);
#7064=AXIS2_PLACEMENT_3D('',#18306,#8422,#8423);
#7065=AXIS2_PLACEMENT_3D('',#18307,#8424,#8425);
#7066=AXIS2_PLACEMENT_3D('',#18308,#8426,#8427);
#7067=AXIS2_PLACEMENT_3D('',#18310,#8428,#8429);
#7068=AXIS2_PLACEMENT_3D('',#18313,#8431,#8432);
#7069=AXIS2_PLACEMENT_3D('',#18314,#8433,#8434);
#7070=AXIS2_PLACEMENT_3D('',#18316,#8435,#8436);
#7071=AXIS2_PLACEMENT_3D('',#18319,#8438,#8439);
#7072=AXIS2_PLACEMENT_3D('',#18320,#8440,#8441);
#7073=AXIS2_PLACEMENT_3D('',#18321,#8442,#8443);
#7074=AXIS2_PLACEMENT_3D('',#18322,#8444,#8445);
#7075=AXIS2_PLACEMENT_3D('',#18323,#8446,#8447);
#7076=AXIS2_PLACEMENT_3D('',#18324,#8448,#8449);
#7077=AXIS2_PLACEMENT_3D('',#18325,#8450,#8451);
#7078=AXIS2_PLACEMENT_3D('',#18326,#8452,#8453);
#7079=AXIS2_PLACEMENT_3D('',#18327,#8454,#8455);
#7080=AXIS2_PLACEMENT_3D('',#18328,#8456,#8457);
#7081=AXIS2_PLACEMENT_3D('',#18329,#8458,#8459);
#7082=DIRECTION('axis',(0.,0.,1.));
#7083=DIRECTION('refdir',(1.,0.,0.));
#7084=DIRECTION('axis',(0.,0.,1.));
#7085=DIRECTION('refdir',(1.,0.,0.));
#7086=DIRECTION('center_axis',(0.,0.,-1.));
#7087=DIRECTION('ref_axis',(1.,0.,0.));
#7088=DIRECTION('center_axis',(0.,0.,-1.));
#7089=DIRECTION('ref_axis',(1.,0.,0.));
#7090=DIRECTION('',(0.,0.,-1.));
#7091=DIRECTION('center_axis',(0.,0.,1.));
#7092=DIRECTION('ref_axis',(1.,0.,0.));
#7093=DIRECTION('center_axis',(0.,0.,-1.));
#7094=DIRECTION('ref_axis',(1.,0.,0.));
#7095=DIRECTION('center_axis',(0.,0.,-1.));
#7096=DIRECTION('ref_axis',(1.,0.,0.));
#7097=DIRECTION('',(0.,0.,-1.));
#7098=DIRECTION('center_axis',(0.,0.,1.));
#7099=DIRECTION('ref_axis',(1.,0.,0.));
#7100=DIRECTION('center_axis',(0.,0.,-1.));
#7101=DIRECTION('ref_axis',(1.,0.,0.));
#7102=DIRECTION('center_axis',(0.,0.,-1.));
#7103=DIRECTION('ref_axis',(1.,0.,0.));
#7104=DIRECTION('',(0.,0.,-1.));
#7105=DIRECTION('center_axis',(0.,0.,1.));
#7106=DIRECTION('ref_axis',(1.,0.,0.));
#7107=DIRECTION('center_axis',(0.852825510654705,0.52219598655729,2.98280813317006E-15));
#7108=DIRECTION('ref_axis',(-2.45173672180486E-15,-1.70798806265451E-15,
1.));
#7109=DIRECTION('',(0.52219598655729,-0.852825510654705,0.));
#7110=DIRECTION('',(-0.417756789245834,0.682260408523763,0.600000000000001));
#7111=DIRECTION('',(0.,0.,1.));
#7112=DIRECTION('center_axis',(0.,0.,-1.));
#7113=DIRECTION('ref_axis',(-0.52219598655729,-0.852825510654705,0.));
#7114=DIRECTION('',(0.417756789245831,0.682260408523765,0.600000000000001));
#7115=DIRECTION('center_axis',(0.,0.,1.));
#7116=DIRECTION('ref_axis',(-0.52219598655729,-0.852825510654705,0.));
#7117=DIRECTION('center_axis',(0.,0.,1.));
#7118=DIRECTION('ref_axis',(-0.52219598655729,-0.852825510654705,0.));
#7119=DIRECTION('center_axis',(0.852825510654705,-0.52219598655729,2.98280813317006E-15));
#7120=DIRECTION('ref_axis',(-2.63589301690668E-15,1.4072328089692E-15,1.));
#7121=DIRECTION('',(0.52219598655729,0.852825510654705,0.));
#7122=DIRECTION('',(0.,0.,1.));
#7123=DIRECTION('center_axis',(0.8,-0.6,0.));
#7124=DIRECTION('ref_axis',(0.6,0.8,0.));
#7125=DIRECTION('',(0.,0.,-1.));
#7126=DIRECTION('',(0.6,0.8,0.));
#7127=DIRECTION('',(-0.6,-0.8,0.));
#7128=DIRECTION('center_axis',(0.242535625036333,0.970142500145332,0.));
#7129=DIRECTION('ref_axis',(-0.970142500145332,0.242535625036333,0.));
#7130=DIRECTION('',(0.970142500145332,-0.242535625036333,0.));
#7131=DIRECTION('',(0.,0.,1.));
#7132=DIRECTION('',(-0.970142500145332,0.242535625036333,0.));
#7133=DIRECTION('',(0.,0.,1.));
#7134=DIRECTION('center_axis',(0.,0.,1.));
#7135=DIRECTION('ref_axis',(4.44089209850063E-15,1.,0.));
#7136=DIRECTION('center_axis',(0.,0.,1.));
#7137=DIRECTION('ref_axis',(4.44089209850063E-15,1.,0.));
#7138=DIRECTION('center_axis',(0.,0.,1.));
#7139=DIRECTION('ref_axis',(4.44089209850063E-15,1.,0.));
#7140=DIRECTION('',(0.,0.,1.));
#7141=DIRECTION('center_axis',(0.,0.,1.));
#7142=DIRECTION('ref_axis',(-0.0764170008251969,0.997075945946387,0.));
#7143=DIRECTION('center_axis',(0.,0.,1.));
#7144=DIRECTION('ref_axis',(-0.0764170008251969,0.997075945946387,0.));
#7145=DIRECTION('center_axis',(0.,0.,1.));
#7146=DIRECTION('ref_axis',(-0.0764170008251969,0.997075945946387,0.));
#7147=DIRECTION('center_axis',(0.,0.,1.));
#7148=DIRECTION('ref_axis',(1.,0.,0.));
#7149=DIRECTION('',(0.,-1.,0.));
#7150=DIRECTION('',(-1.,0.,0.));
#7151=DIRECTION('center_axis',(0.,1.,0.));
#7152=DIRECTION('ref_axis',(-1.,0.,0.));
#7153=DIRECTION('',(0.,0.,1.));
#7154=DIRECTION('',(-1.,0.,0.));
#7155=DIRECTION('',(0.,0.,1.));
#7156=DIRECTION('',(1.,0.,0.));
#7157=DIRECTION('center_axis',(-1.,0.,0.));
#7158=DIRECTION('ref_axis',(0.,-1.,0.));
#7159=DIRECTION('',(0.,1.,0.));
#7160=DIRECTION('',(0.,0.,1.));
#7161=DIRECTION('',(0.,-1.,0.));
#7162=DIRECTION('center_axis',(0.,-1.,0.));
#7163=DIRECTION('ref_axis',(1.,0.,0.));
#7164=DIRECTION('',(0.,0.,-1.));
#7165=DIRECTION('',(1.,0.,0.));
#7166=DIRECTION('',(-1.,0.,0.));
#7167=DIRECTION('center_axis',(1.,0.,0.));
#7168=DIRECTION('ref_axis',(0.,1.,0.));
#7169=DIRECTION('',(0.,0.,1.));
#7170=DIRECTION('',(0.,-1.,0.));
#7171=DIRECTION('',(0.,1.,0.));
#7172=DIRECTION('center_axis',(0.,0.,1.));
#7173=DIRECTION('ref_axis',(1.,0.,0.));
#7174=DIRECTION('center_axis',(0.,0.,1.));
#7175=DIRECTION('ref_axis',(1.,0.,0.));
#7176=DIRECTION('',(0.,0.,1.));
#7177=DIRECTION('center_axis',(0.,0.,1.));
#7178=DIRECTION('ref_axis',(1.,0.,0.));
#7179=DIRECTION('center_axis',(0.,0.,1.));
#7180=DIRECTION('ref_axis',(1.,0.,0.));
#7181=DIRECTION('center_axis',(0.,0.,1.));
#7182=DIRECTION('ref_axis',(1.,0.,0.));
#7183=DIRECTION('',(0.,0.,-1.));
#7184=DIRECTION('center_axis',(0.,0.,1.));
#7185=DIRECTION('ref_axis',(1.,0.,0.));
#7186=DIRECTION('center_axis',(0.,0.,1.));
#7187=DIRECTION('ref_axis',(1.,0.,0.));
#7188=DIRECTION('',(0.87524153543927,-0.483686111690123,0.));
#7189=DIRECTION('center_axis',(0.,0.,1.));
#7190=DIRECTION('ref_axis',(1.,0.,0.));
#7191=DIRECTION('',(0.87524153543927,-0.483686111690123,0.));
#7192=DIRECTION('',(1.,0.,0.));
#7193=DIRECTION('',(0.,1.,0.));
#7194=DIRECTION('',(-1.,0.,0.));
#7195=DIRECTION('',(-0.694594513699567,0.719401460617409,0.));
#7196=DIRECTION('center_axis',(0.,0.,1.));
#7197=DIRECTION('ref_axis',(1.,0.,0.));
#7198=DIRECTION('',(-0.694594513699567,0.719401460617409,0.));
#7199=DIRECTION('',(-0.447213595499958,-0.894427190999916,0.));
#7200=DIRECTION('center_axis',(0.,0.,1.));
#7201=DIRECTION('ref_axis',(-1.,0.,0.));
#7202=DIRECTION('center_axis',(0.,0.,1.));
#7203=DIRECTION('ref_axis',(1.,0.,0.));
#7204=DIRECTION('center_axis',(0.,0.,-1.));
#7205=DIRECTION('ref_axis',(-1.,2.01858731750028E-16,0.));
#7206=DIRECTION('center_axis',(0.,-1.,0.));
#7207=DIRECTION('ref_axis',(-1.,0.,0.));
#7208=DIRECTION('center_axis',(0.,0.,1.));
#7209=DIRECTION('ref_axis',(-1.,2.01858731750028E-16,0.));
#7210=DIRECTION('center_axis',(0.,0.,-1.));
#7211=DIRECTION('ref_axis',(1.,0.,0.));
#7212=DIRECTION('center_axis',(0.,0.,-1.));
#7213=DIRECTION('ref_axis',(-1.,0.,0.));
#7214=DIRECTION('center_axis',(0.,0.,-1.));
#7215=DIRECTION('ref_axis',(-1.,0.,0.));
#7216=DIRECTION('',(0.,0.,-1.));
#7217=DIRECTION('center_axis',(0.,0.,1.));
#7218=DIRECTION('ref_axis',(1.,0.,0.));
#7219=DIRECTION('',(-0.447213595499958,-0.894427190999916,0.));
#7220=DIRECTION('',(-0.694594513699567,0.719401460617409,0.));
#7221=DIRECTION('center_axis',(0.,0.,1.));
#7222=DIRECTION('ref_axis',(1.,0.,0.));
#7223=DIRECTION('',(-0.694594513699567,0.719401460617409,0.));
#7224=DIRECTION('',(-1.,0.,0.));
#7225=DIRECTION('',(0.,1.,0.));
#7226=DIRECTION('',(1.,0.,0.));
#7227=DIRECTION('',(0.87524153543927,-0.483686111690123,0.));
#7228=DIRECTION('center_axis',(0.,0.,1.));
#7229=DIRECTION('ref_axis',(1.,0.,0.));
#7230=DIRECTION('',(0.87524153543927,-0.483686111690123,0.));
#7231=DIRECTION('center_axis',(0.,0.,-1.));
#7232=DIRECTION('ref_axis',(-1.,0.,0.));
#7233=DIRECTION('center_axis',(0.,-1.,0.));
#7234=DIRECTION('ref_axis',(1.,0.,0.));
#7235=DIRECTION('center_axis',(0.,0.,1.));
#7236=DIRECTION('ref_axis',(1.,0.,0.));
#7237=DIRECTION('',(0.,0.,-1.));
#7238=DIRECTION('',(0.,0.,1.));
#7239=DIRECTION('center_axis',(0.,0.,1.));
#7240=DIRECTION('ref_axis',(-0.483686111690122,-0.87524153543927,0.));
#7241=DIRECTION('',(0.,0.,1.));
#7242=DIRECTION('',(0.,0.,-1.));
#7243=DIRECTION('center_axis',(-0.483686111690123,-0.87524153543927,0.));
#7244=DIRECTION('ref_axis',(0.87524153543927,-0.483686111690123,0.));
#7245=DIRECTION('',(0.,0.,1.));
#7246=DIRECTION('center_axis',(0.719401460617409,0.694594513699567,0.));
#7247=DIRECTION('ref_axis',(-0.694594513699567,0.719401460617409,0.));
#7248=DIRECTION('',(0.,0.,1.));
#7249=DIRECTION('center_axis',(-0.483686111690123,-0.87524153543927,0.));
#7250=DIRECTION('ref_axis',(0.87524153543927,-0.483686111690123,0.));
#7251=DIRECTION('center_axis',(-0.894427190999916,0.447213595499958,0.));
#7252=DIRECTION('ref_axis',(-0.447213595499958,-0.894427190999916,0.));
#7253=DIRECTION('',(0.,0.,1.));
#7254=DIRECTION('center_axis',(0.719401460617409,0.694594513699567,0.));
#7255=DIRECTION('ref_axis',(-0.694594513699567,0.719401460617409,0.));
#7256=DIRECTION('center_axis',(0.,1.,0.));
#7257=DIRECTION('ref_axis',(-1.,0.,0.));
#7258=DIRECTION('',(0.,0.,1.));
#7259=DIRECTION('center_axis',(1.,0.,0.));
#7260=DIRECTION('ref_axis',(0.,1.,0.));
#7261=DIRECTION('',(0.,0.,1.));
#7262=DIRECTION('center_axis',(0.,-1.,0.));
#7263=DIRECTION('ref_axis',(1.,0.,0.));
#7264=DIRECTION('axis',(0.,0.,1.));
#7265=DIRECTION('refdir',(1.,0.,0.));
#7266=DIRECTION('center_axis',(0.,0.,1.));
#7267=DIRECTION('ref_axis',(1.,0.,0.));
#7268=DIRECTION('center_axis',(0.,0.,1.));
#7269=DIRECTION('ref_axis',(1.,0.,0.));
#7270=DIRECTION('',(0.,0.,1.));
#7271=DIRECTION('center_axis',(0.,0.,1.));
#7272=DIRECTION('ref_axis',(1.,0.,0.));
#7273=DIRECTION('center_axis',(0.,0.,-1.));
#7274=DIRECTION('ref_axis',(-1.,0.,0.));
#7275=DIRECTION('center_axis',(0.,0.,-1.));
#7276=DIRECTION('ref_axis',(1.,0.,0.));
#7277=DIRECTION('center_axis',(0.,0.,1.));
#7278=DIRECTION('ref_axis',(1.,0.,0.));
#7279=DIRECTION('center_axis',(0.,0.,1.));
#7280=DIRECTION('ref_axis',(1.,0.,0.));
#7281=DIRECTION('center_axis',(0.,0.,1.));
#7282=DIRECTION('ref_axis',(1.,0.,0.));
#7283=DIRECTION('center_axis',(0.,0.,1.));
#7284=DIRECTION('ref_axis',(1.,0.,0.));
#7285=DIRECTION('',(0.,0.,-1.));
#7286=DIRECTION('center_axis',(0.,0.,1.));
#7287=DIRECTION('ref_axis',(1.,0.,0.));
#7288=DIRECTION('center_axis',(0.,0.,1.));
#7289=DIRECTION('ref_axis',(1.,0.,0.));
#7290=DIRECTION('center_axis',(0.,0.,1.));
#7291=DIRECTION('ref_axis',(1.,0.,0.));
#7292=DIRECTION('center_axis',(0.,0.,1.));
#7293=DIRECTION('ref_axis',(1.,0.,0.));
#7294=DIRECTION('',(0.,0.,-1.));
#7295=DIRECTION('center_axis',(0.,0.,1.));
#7296=DIRECTION('ref_axis',(1.,0.,0.));
#7297=DIRECTION('center_axis',(0.,0.,1.));
#7298=DIRECTION('ref_axis',(1.,0.,0.));
#7299=DIRECTION('center_axis',(0.,0.,1.));
#7300=DIRECTION('ref_axis',(1.,0.,0.));
#7301=DIRECTION('',(0.,0.,-1.));
#7302=DIRECTION('center_axis',(0.,0.,1.));
#7303=DIRECTION('ref_axis',(1.,0.,0.));
#7304=DIRECTION('axis',(0.,0.,1.));
#7305=DIRECTION('refdir',(1.,0.,0.));
#7306=DIRECTION('center_axis',(-1.,0.,0.));
#7307=DIRECTION('ref_axis',(0.,1.,0.));
#7308=DIRECTION('',(0.,0.,1.));
#7309=DIRECTION('',(0.,-1.,0.));
#7310=DIRECTION('',(0.,0.,-1.));
#7311=DIRECTION('',(0.,1.,0.));
#7312=DIRECTION('center_axis',(1.,0.,0.));
#7313=DIRECTION('ref_axis',(0.,-1.,0.));
#7314=DIRECTION('',(0.,0.,-1.));
#7315=DIRECTION('',(0.,-1.,0.));
#7316=DIRECTION('',(0.,0.,1.));
#7317=DIRECTION('',(0.,1.,0.));
#7318=DIRECTION('center_axis',(0.,0.,1.));
#7319=DIRECTION('ref_axis',(1.,0.,0.));
#7320=DIRECTION('center_axis',(0.,0.,1.));
#7321=DIRECTION('ref_axis',(1.,0.,0.));
#7322=DIRECTION('center_axis',(0.,0.,-1.));
#7323=DIRECTION('ref_axis',(1.,0.,0.));
#7324=DIRECTION('center_axis',(0.,0.,1.));
#7325=DIRECTION('ref_axis',(6.12323399573677E-17,-1.,0.));
#7326=DIRECTION('center_axis',(0.,0.,-1.));
#7327=DIRECTION('ref_axis',(1.,0.,0.));
#7328=DIRECTION('center_axis',(0.,0.,1.));
#7329=DIRECTION('ref_axis',(6.12323399573677E-17,-1.,0.));
#7330=DIRECTION('center_axis',(0.,0.,1.));
#7331=DIRECTION('ref_axis',(1.,0.,0.));
#7332=DIRECTION('center_axis',(0.,0.,1.));
#7333=DIRECTION('ref_axis',(1.,0.,0.));
#7334=DIRECTION('axis',(0.,0.,1.));
#7335=DIRECTION('refdir',(1.,0.,0.));
#7336=DIRECTION('axis',(0.,0.,1.));
#7337=DIRECTION('refdir',(1.,0.,0.));
#7338=DIRECTION('center_axis',(0.,0.,-1.));
#7339=DIRECTION('ref_axis',(1.,0.,0.));
#7340=DIRECTION('center_axis',(1.01338750660366E-31,-1.26069923670246E-19,
-1.));
#7341=DIRECTION('ref_axis',(1.,0.,0.));
#7342=DIRECTION('',(0.,0.,-1.));
#7343=DIRECTION('center_axis',(-1.01338750660366E-31,1.26069923670246E-19,
1.));
#7344=DIRECTION('ref_axis',(1.,0.,0.));
#7345=DIRECTION('center_axis',(0.,0.,-1.));
#7346=DIRECTION('ref_axis',(1.,0.,0.));
#7347=DIRECTION('center_axis',(1.01338750660366E-31,-1.26069923670246E-19,
-1.));
#7348=DIRECTION('ref_axis',(1.,0.,0.));
#7349=DIRECTION('',(0.,0.,-1.));
#7350=DIRECTION('center_axis',(-1.01338750660366E-31,1.26069923670246E-19,
1.));
#7351=DIRECTION('ref_axis',(1.,0.,0.));
#7352=DIRECTION('center_axis',(0.,0.,-1.));
#7353=DIRECTION('ref_axis',(1.,0.,0.));
#7354=DIRECTION('center_axis',(1.01338750660366E-31,-1.26069923670246E-19,
-1.));
#7355=DIRECTION('ref_axis',(1.,0.,0.));
#7356=DIRECTION('',(0.,0.,-1.));
#7357=DIRECTION('center_axis',(-1.01338750660366E-31,1.26069923670246E-19,
1.));
#7358=DIRECTION('ref_axis',(1.,0.,0.));
#7359=DIRECTION('center_axis',(0.,0.,-1.));
#7360=DIRECTION('ref_axis',(1.,0.,0.));
#7361=DIRECTION('center_axis',(1.01338750660366E-31,-1.26069923670246E-19,
-1.));
#7362=DIRECTION('ref_axis',(1.,0.,0.));
#7363=DIRECTION('',(0.,0.,-1.));
#7364=DIRECTION('center_axis',(-1.01338750660366E-31,1.26069923670246E-19,
1.));
#7365=DIRECTION('ref_axis',(1.,0.,0.));
#7366=DIRECTION('center_axis',(0.,0.,-1.));
#7367=DIRECTION('ref_axis',(1.,0.,0.));
#7368=DIRECTION('center_axis',(1.01338750660366E-31,-1.26069923670246E-19,
-1.));
#7369=DIRECTION('ref_axis',(1.,0.,0.));
#7370=DIRECTION('',(0.,0.,-1.));
#7371=DIRECTION('center_axis',(0.,0.,-1.));
#7372=DIRECTION('ref_axis',(1.,0.,0.));
#7373=DIRECTION('center_axis',(0.,0.,-1.));
#7374=DIRECTION('ref_axis',(1.,0.,0.));
#7375=DIRECTION('center_axis',(0.,0.,1.));
#7376=DIRECTION('ref_axis',(1.,0.,0.));
#7377=DIRECTION('center_axis',(0.,0.,-1.));
#7378=DIRECTION('ref_axis',(1.,0.,0.));
#7379=DIRECTION('center_axis',(1.01338750660366E-31,-1.26069923670246E-19,
-1.));
#7380=DIRECTION('ref_axis',(1.,0.,0.));
#7381=DIRECTION('',(0.,0.,-1.));
#7382=DIRECTION('center_axis',(0.,0.,-1.));
#7383=DIRECTION('ref_axis',(1.,0.,0.));
#7384=DIRECTION('center_axis',(0.,0.,-1.));
#7385=DIRECTION('ref_axis',(1.,0.,0.));
#7386=DIRECTION('center_axis',(0.,0.,1.));
#7387=DIRECTION('ref_axis',(1.,0.,0.));
#7388=DIRECTION('center_axis',(0.,0.,-1.));
#7389=DIRECTION('ref_axis',(1.,0.,0.));
#7390=DIRECTION('',(0.,0.,-1.));
#7391=DIRECTION('center_axis',(0.,0.,1.));
#7392=DIRECTION('ref_axis',(1.,0.,0.));
#7393=DIRECTION('center_axis',(0.,0.,-1.));
#7394=DIRECTION('ref_axis',(1.,0.,0.));
#7395=DIRECTION('',(0.,0.,-1.));
#7396=DIRECTION('center_axis',(0.,0.,1.));
#7397=DIRECTION('ref_axis',(1.,0.,0.));
#7398=DIRECTION('center_axis',(0.,-1.,0.));
#7399=DIRECTION('ref_axis',(-1.,0.,0.));
#7400=DIRECTION('',(0.0523359562429438,0.,0.998629534754574));
#7401=DIRECTION('',(1.,0.,0.));
#7402=DIRECTION('',(-0.0523359562429438,0.,-0.998629534754574));
#7403=DIRECTION('',(1.,0.,0.));
#7404=DIRECTION('center_axis',(0.,-1.,0.));
#7405=DIRECTION('ref_axis',(-1.,0.,0.));
#7406=DIRECTION('',(0.,0.,-1.));
#7407=DIRECTION('',(1.,0.,0.));
#7408=DIRECTION('',(0.,0.,1.));
#7409=DIRECTION('',(1.,0.,0.));
#7410=DIRECTION('center_axis',(0.,-1.,0.));
#7411=DIRECTION('ref_axis',(-1.,0.,0.));
#7412=DIRECTION('',(0.,0.,-1.));
#7413=DIRECTION('',(1.,0.,0.));
#7414=DIRECTION('',(0.,0.,1.));
#7415=DIRECTION('',(1.,0.,0.));
#7416=DIRECTION('center_axis',(0.,-1.,0.));
#7417=DIRECTION('ref_axis',(-1.,0.,0.));
#7418=DIRECTION('',(0.,0.,-1.));
#7419=DIRECTION('',(1.,0.,0.));
#7420=DIRECTION('',(0.,0.,1.));
#7421=DIRECTION('',(1.,0.,0.));
#7422=DIRECTION('center_axis',(0.,1.,0.));
#7423=DIRECTION('ref_axis',(1.,0.,0.));
#7424=DIRECTION('',(-0.0523359562429438,0.,-0.998629534754574));
#7425=DIRECTION('',(-1.,0.,0.));
#7426=DIRECTION('',(0.0523359562429438,0.,0.998629534754574));
#7427=DIRECTION('',(-1.,0.,0.));
#7428=DIRECTION('center_axis',(0.,1.,0.));
#7429=DIRECTION('ref_axis',(1.,0.,0.));
#7430=DIRECTION('',(0.,0.,1.));
#7431=DIRECTION('',(-1.,0.,0.));
#7432=DIRECTION('',(0.,0.,-1.));
#7433=DIRECTION('',(-1.,0.,0.));
#7434=DIRECTION('center_axis',(0.,1.,0.));
#7435=DIRECTION('ref_axis',(1.,0.,0.));
#7436=DIRECTION('',(0.,0.,1.));
#7437=DIRECTION('',(-1.,0.,0.));
#7438=DIRECTION('',(0.,0.,-1.));
#7439=DIRECTION('',(-1.,0.,0.));
#7440=DIRECTION('center_axis',(0.,0.,1.));
#7441=DIRECTION('ref_axis',(1.,0.,0.));
#7442=DIRECTION('center_axis',(0.,0.,1.));
#7443=DIRECTION('ref_axis',(1.,0.,0.));
#7444=DIRECTION('center_axis',(0.,0.,1.));
#7445=DIRECTION('ref_axis',(1.,0.,0.));
#7446=DIRECTION('center_axis',(0.,0.,1.));
#7447=DIRECTION('ref_axis',(1.,0.,0.));
#7448=DIRECTION('center_axis',(0.,0.,1.));
#7449=DIRECTION('ref_axis',(1.,0.,0.));
#7450=DIRECTION('',(0.,1.,0.));
#7451=DIRECTION('',(0.,-1.,0.));
#7452=DIRECTION('center_axis',(0.,0.,1.));
#7453=DIRECTION('ref_axis',(1.,0.,0.));
#7454=DIRECTION('',(0.,-1.,0.));
#7455=DIRECTION('',(0.,1.,0.));
#7456=DIRECTION('center_axis',(0.,0.,1.));
#7457=DIRECTION('ref_axis',(1.,0.,0.));
#7458=DIRECTION('',(0.,-1.,0.));
#7459=DIRECTION('',(0.,1.,0.));
#7460=DIRECTION('center_axis',(0.,0.,1.));
#7461=DIRECTION('ref_axis',(1.,0.,0.));
#7462=DIRECTION('',(0.,-1.,0.));
#7463=DIRECTION('',(-1.,0.,0.));
#7464=DIRECTION('',(0.,1.,0.));
#7465=DIRECTION('center_axis',(0.,1.,0.));
#7466=DIRECTION('ref_axis',(1.,0.,0.));
#7467=DIRECTION('',(0.,0.,1.));
#7468=DIRECTION('',(-1.,0.,0.));
#7469=DIRECTION('',(0.,0.,-1.));
#7470=DIRECTION('center_axis',(-1.,0.,0.));
#7471=DIRECTION('ref_axis',(0.,-1.,0.));
#7472=DIRECTION('',(0.,-1.,0.));
#7473=DIRECTION('',(0.,-1.,1.26069923670246E-19));
#7474=DIRECTION('center_axis',(1.,0.,0.));
#7475=DIRECTION('ref_axis',(0.,1.,0.));
#7476=DIRECTION('',(0.,1.,0.));
#7477=DIRECTION('',(0.,1.,-1.26069923670246E-19));
#7478=DIRECTION('',(0.,1.,0.));
#7479=DIRECTION('center_axis',(1.,0.,0.));
#7480=DIRECTION('ref_axis',(0.,1.,0.));
#7481=DIRECTION('',(0.,1.,0.));
#7482=DIRECTION('',(0.,1.,-1.26069923670246E-19));
#7483=DIRECTION('',(0.,1.,0.));
#7484=DIRECTION('center_axis',(1.,0.,0.));
#7485=DIRECTION('ref_axis',(0.,1.,0.));
#7486=DIRECTION('',(0.,1.,0.));
#7487=DIRECTION('',(0.,1.,-1.26069923670246E-19));
#7488=DIRECTION('',(0.,1.,0.));
#7489=DIRECTION('center_axis',(0.998629534754574,0.,-0.0523359562429438));
#7490=DIRECTION('ref_axis',(-0.0523359562429438,0.,-0.998629534754574));
#7491=DIRECTION('',(0.,-1.,0.));
#7492=DIRECTION('',(6.6070447339401E-21,-1.,1.26069923670246E-19));
#7493=DIRECTION('',(0.,-1.,0.));
#7494=DIRECTION('center_axis',(0.,0.,1.));
#7495=DIRECTION('ref_axis',(1.,0.,0.));
#7496=DIRECTION('',(0.,-1.,0.));
#7497=DIRECTION('',(0.,-1.,0.));
#7498=DIRECTION('',(0.,-1.,0.));
#7499=DIRECTION('',(0.,1.,0.));
#7500=DIRECTION('',(0.,-1.,0.));
#7501=DIRECTION('',(0.,1.,0.));
#7502=DIRECTION('',(0.,-1.,0.));
#7503=DIRECTION('',(0.,-1.,0.));
#7504=DIRECTION('',(0.,-1.,0.));
#7505=DIRECTION('',(0.,1.,0.));
#7506=DIRECTION('',(0.,1.,0.));
#7507=DIRECTION('center_axis',(0.,0.,1.));
#7508=DIRECTION('ref_axis',(1.,0.,0.));
#7509=DIRECTION('center_axis',(-1.01338750660366E-31,1.26069923670246E-19,
1.));
#7510=DIRECTION('ref_axis',(1.,0.,0.));
#7511=DIRECTION('',(0.,0.,-1.));
#7512=DIRECTION('center_axis',(0.,0.,1.));
#7513=DIRECTION('ref_axis',(1.,0.,0.));
#7514=DIRECTION('center_axis',(-1.01338750660366E-31,1.26069923670246E-19,
1.));
#7515=DIRECTION('ref_axis',(1.,0.,0.));
#7516=DIRECTION('',(0.,0.,-1.));
#7517=DIRECTION('center_axis',(1.,0.,0.));
#7518=DIRECTION('ref_axis',(0.,1.,0.));
#7519=DIRECTION('',(0.,1.,-1.26069923670246E-19));
#7520=DIRECTION('center_axis',(0.995216631131787,0.0976926666577189,1.18580395612125E-14));
#7521=DIRECTION('ref_axis',(0.0975341006448478,-0.993601284365854,0.0569524970297685));
#7522=DIRECTION('center_axis',(-1.01338750660366E-31,1.26069923670246E-19,
1.));
#7523=DIRECTION('ref_axis',(1.,0.,1.01338750660366E-31));
#7524=DIRECTION('center_axis',(-1.01338750660366E-31,1.26069923670246E-19,
1.));
#7525=DIRECTION('ref_axis',(1.,0.,1.01338750660366E-31));
#7526=DIRECTION('',(-6.60704473394009E-21,-1.,1.26069923670246E-19));
#7527=DIRECTION('center_axis',(-1.,0.,0.));
#7528=DIRECTION('ref_axis',(0.,-1.,0.));
#7529=DIRECTION('',(0.,-1.,1.26069923670246E-19));
#7530=DIRECTION('center_axis',(-1.01338750660366E-31,1.26069923670246E-19,
1.));
#7531=DIRECTION('ref_axis',(1.,0.,1.01338750660366E-31));
#7532=DIRECTION('center_axis',(-1.,0.,0.));
#7533=DIRECTION('ref_axis',(0.,-1.,0.));
#7534=DIRECTION('',(0.,-1.,1.26069923670246E-19));
#7535=DIRECTION('center_axis',(-1.01338750660366E-31,1.26069923670246E-19,
1.));
#7536=DIRECTION('ref_axis',(1.,0.,1.01338750660366E-31));
#7537=DIRECTION('center_axis',(-1.,0.,0.));
#7538=DIRECTION('ref_axis',(0.,-1.,0.));
#7539=DIRECTION('',(0.,-1.,1.26069923670246E-19));
#7540=DIRECTION('center_axis',(-0.982258063247475,0.187534256031586,1.45403402392141E-15));
#7541=DIRECTION('ref_axis',(1.48029736616688E-15,0.,1.));
#7542=DIRECTION('center_axis',(-1.01338750660366E-31,1.26069923670246E-19,
1.));
#7543=DIRECTION('ref_axis',(1.,0.,1.01338750660366E-31));
#7544=DIRECTION('',(-6.6070447339401E-21,1.,-1.26069923670246E-19));
#7545=DIRECTION('center_axis',(-0.982258063247479,-0.187534256031562,9.14061384143289E-15));
#7546=DIRECTION('ref_axis',(-0.187187393251729,0.980441281772238,0.0607928680392112));
#7547=DIRECTION('center_axis',(-0.45173408531537,0.373496730537872,-0.810207694632559));
#7548=DIRECTION('ref_axis',(-0.624418441188311,0.516273298501642,0.586142893463867));
#7549=DIRECTION('center_axis',(-2.96465769266614E-15,1.,0.));
#7550=DIRECTION('ref_axis',(0.,0.,1.));
#7551=DIRECTION('center_axis',(0.0522655346583812,-0.0518587053130894,0.997285810873755));
#7552=DIRECTION('ref_axis',(-0.998629534754574,0.,0.0523359562429445));
#7553=DIRECTION('center_axis',(0.377681861983732,-0.843372107574977,0.38220400219391));
#7554=DIRECTION('ref_axis',(0.592794689304902,0.537329962094562,0.599892463836113));
#7555=DIRECTION('center_axis',(0.995216631131786,-0.0976926666577302,0.));
#7556=DIRECTION('ref_axis',(0.,0.,1.));
#7557=DIRECTION('center_axis',(-0.0522650609395843,-0.052032719242908,0.997276771780618));
#7558=DIRECTION('ref_axis',(0.0975341006448596,0.993601284365853,0.0569524970297681));
#7559=DIRECTION('center_axis',(1.55158195278682E-16,1.,-2.96059473233375E-15));
#7560=DIRECTION('ref_axis',(0.998629534754574,0.,0.0523359562429438));
#7561=DIRECTION('center_axis',(-0.45173408531537,-0.373496730537869,-0.810207694632561));
#7562=DIRECTION('ref_axis',(-0.624418441188315,-0.516273298501641,0.586142893463864));
#7563=DIRECTION('center_axis',(0.0522655346583823,0.0518587053130918,0.997285810873755));
#7564=DIRECTION('ref_axis',(-0.187187393251729,-0.980441281772238,0.0607928680392122));
#7565=DIRECTION('center_axis',(-2.71526841737693E-16,-1.,-5.18104078158406E-15));
#7566=DIRECTION('ref_axis',(-0.998629534754574,0.,0.0523359562429439));
#7567=DIRECTION('center_axis',(-6.6070447339401E-21,1.,-1.26069923670246E-19));
#7568=DIRECTION('ref_axis',(-0.688354575693753,0.,0.725374371012289));
#7569=DIRECTION('center_axis',(-0.377681861983722,-0.843372107574983,-0.382204002193908));
#7570=DIRECTION('ref_axis',(0.592794689304909,-0.537329962094554,0.599892463836112));
#7571=DIRECTION('center_axis',(-0.0522650609395818,0.0520327192429072,0.997276771780618));
#7572=DIRECTION('ref_axis',(0.998629534754574,0.,0.0523359562429431));
#7573=DIRECTION('center_axis',(2.96465769266612E-15,-1.,0.));
#7574=DIRECTION('ref_axis',(0.,0.,1.));
#7575=DIRECTION('center_axis',(-6.60704473394009E-21,-1.,1.26069923670246E-19));
#7576=DIRECTION('ref_axis',(0.688354575693758,0.,0.725374371012284));
#7577=DIRECTION('',(6.60704473394009E-21,1.,-1.26069923670246E-19));
#7578=DIRECTION('center_axis',(-0.998629534754574,0.,-0.0523359562429438));
#7579=DIRECTION('ref_axis',(-0.0523359562429438,0.,0.998629534754574));
#7580=DIRECTION('center_axis',(-0.45173408531537,0.373496730537872,-0.81020769463256));
#7581=DIRECTION('ref_axis',(-0.624418441188311,0.516273298501643,0.586142893463866));
#7582=DIRECTION('center_axis',(-2.96465769266614E-15,1.,0.));
#7583=DIRECTION('ref_axis',(0.,0.,1.));
#7584=DIRECTION('center_axis',(-0.982258063247479,-0.187534256031562,9.14061384143289E-15));
#7585=DIRECTION('ref_axis',(-0.187187393251729,0.980441281772238,0.0607928680392111));
#7586=DIRECTION('center_axis',(0.0522655346583812,-0.0518587053130894,0.997285810873755));
#7587=DIRECTION('ref_axis',(-0.998629534754574,0.,0.0523359562429445));
#7588=DIRECTION('center_axis',(0.377681861983731,-0.843372107574978,0.38220400219391));
#7589=DIRECTION('ref_axis',(0.592794689304906,0.537329962094559,0.599892463836111));
#7590=DIRECTION('center_axis',(0.995216631131786,-0.0976926666577302,0.));
#7591=DIRECTION('ref_axis',(0.,0.,1.));
#7592=DIRECTION('center_axis',(1.55158195278682E-16,1.,-2.96059473233375E-15));
#7593=DIRECTION('ref_axis',(0.998629534754574,0.,0.0523359562429438));
#7594=DIRECTION('center_axis',(-0.0522650609395843,-0.052032719242908,0.997276771780618));
#7595=DIRECTION('ref_axis',(0.0975341006448596,0.993601284365853,0.0569524970297681));
#7596=DIRECTION('center_axis',(-0.45173408531537,-0.373496730537868,-0.810207694632561));
#7597=DIRECTION('ref_axis',(-0.624418441188315,-0.516273298501641,0.586142893463864));
#7598=DIRECTION('center_axis',(-0.982258063247475,0.187534256031586,1.45403402392141E-15));
#7599=DIRECTION('ref_axis',(1.48029736616688E-15,0.,1.));
#7600=DIRECTION('center_axis',(-2.71526841737693E-16,-1.,-5.18104078158406E-15));
#7601=DIRECTION('ref_axis',(-0.998629534754574,0.,0.0523359562429439));
#7602=DIRECTION('center_axis',(0.0522655346583823,0.0518587053130918,0.997285810873755));
#7603=DIRECTION('ref_axis',(-0.187187393251729,-0.980441281772238,0.0607928680392122));
#7604=DIRECTION('center_axis',(-6.6070447339401E-21,1.,-1.26069923670246E-19));
#7605=DIRECTION('ref_axis',(-0.688354575693753,0.,0.725374371012289));
#7606=DIRECTION('',(6.6070447339401E-21,-1.,1.26069923670246E-19));
#7607=DIRECTION('',(-6.6070447339401E-21,1.,-1.26069923670246E-19));
#7608=DIRECTION('center_axis',(-0.377681861983727,-0.843372107574981,-0.382204002193907));
#7609=DIRECTION('ref_axis',(0.592794689304909,-0.537329962094554,0.599892463836112));
#7610=DIRECTION('center_axis',(-0.0522650609395818,0.0520327192429072,0.997276771780618));
#7611=DIRECTION('ref_axis',(0.998629534754574,0.,0.0523359562429431));
#7612=DIRECTION('center_axis',(2.96465769266612E-15,-1.,0.));
#7613=DIRECTION('ref_axis',(0.,0.,1.));
#7614=DIRECTION('center_axis',(0.995216631131787,0.0976926666577189,1.18580395612125E-14));
#7615=DIRECTION('ref_axis',(0.0975341006448478,-0.993601284365854,0.0569524970297685));
#7616=DIRECTION('center_axis',(-6.60704473394009E-21,-1.,1.26069923670246E-19));
#7617=DIRECTION('ref_axis',(0.688354575693758,0.,0.725374371012284));
#7618=DIRECTION('',(6.60704473394009E-21,1.,-1.26069923670246E-19));
#7619=DIRECTION('',(-6.60704473394009E-21,-1.,1.26069923670246E-19));
#7620=DIRECTION('center_axis',(0.998629534754574,0.,-0.0523359562429438));
#7621=DIRECTION('ref_axis',(-0.0523359562429438,0.,-0.998629534754574));
#7622=DIRECTION('center_axis',(-1.01338750660366E-31,1.26069923670246E-19,
1.));
#7623=DIRECTION('ref_axis',(1.,0.,1.01338750660366E-31));
#7624=DIRECTION('center_axis',(-0.998629534754574,0.,-0.0523359562429438));
#7625=DIRECTION('ref_axis',(-0.0523359562429438,0.,0.998629534754574));
#7626=DIRECTION('axis',(0.,0.,1.));
#7627=DIRECTION('refdir',(1.,0.,0.));
#7628=DIRECTION('center_axis',(0.,0.,-1.));
#7629=DIRECTION('ref_axis',(1.,0.,0.));
#7630=DIRECTION('center_axis',(1.01338750660366E-31,-1.26069923670246E-19,
-1.));
#7631=DIRECTION('ref_axis',(1.,0.,0.));
#7632=DIRECTION('',(0.,0.,-1.));
#7633=DIRECTION('center_axis',(-1.01338750660366E-31,1.26069923670246E-19,
1.));
#7634=DIRECTION('ref_axis',(1.,0.,0.));
#7635=DIRECTION('center_axis',(0.,0.,-1.));
#7636=DIRECTION('ref_axis',(1.,0.,0.));
#7637=DIRECTION('center_axis',(1.01338750660366E-31,-1.26069923670246E-19,
-1.));
#7638=DIRECTION('ref_axis',(1.,0.,0.));
#7639=DIRECTION('',(0.,0.,-1.));
#7640=DIRECTION('center_axis',(-1.01338750660366E-31,1.26069923670246E-19,
1.));
#7641=DIRECTION('ref_axis',(1.,0.,0.));
#7642=DIRECTION('center_axis',(0.,0.,-1.));
#7643=DIRECTION('ref_axis',(1.,0.,0.));
#7644=DIRECTION('center_axis',(1.01338750660366E-31,-1.26069923670246E-19,
-1.));
#7645=DIRECTION('ref_axis',(1.,0.,0.));
#7646=DIRECTION('',(0.,0.,-1.));
#7647=DIRECTION('center_axis',(-1.01338750660366E-31,1.26069923670246E-19,
1.));
#7648=DIRECTION('ref_axis',(1.,0.,0.));
#7649=DIRECTION('center_axis',(0.,0.,-1.));
#7650=DIRECTION('ref_axis',(1.,0.,0.));
#7651=DIRECTION('center_axis',(1.01338750660366E-31,-1.26069923670246E-19,
-1.));
#7652=DIRECTION('ref_axis',(1.,0.,0.));
#7653=DIRECTION('',(0.,0.,-1.));
#7654=DIRECTION('center_axis',(-1.01338750660366E-31,1.26069923670246E-19,
1.));
#7655=DIRECTION('ref_axis',(1.,0.,0.));
#7656=DIRECTION('center_axis',(0.86602540378444,0.499999999999998,0.));
#7657=DIRECTION('ref_axis',(0.499999999999998,-0.86602540378444,0.));
#7658=DIRECTION('',(0.499999999999998,-0.86602540378444,1.09179756551649E-19));
#7659=DIRECTION('',(0.,0.,-1.));
#7660=DIRECTION('',(0.499999999999998,-0.86602540378444,0.));
#7661=DIRECTION('',(0.,0.,-1.));
#7662=DIRECTION('center_axis',(1.60246890531963E-16,1.,0.));
#7663=DIRECTION('ref_axis',(1.,-1.60246890531963E-16,0.));
#7664=DIRECTION('',(1.,-1.60246890531963E-16,1.01358952973624E-31));
#7665=DIRECTION('',(0.,0.,-1.));
#7666=DIRECTION('',(1.,-1.60246890531963E-16,0.));
#7667=DIRECTION('center_axis',(-0.86602540378444,0.499999999999998,0.));
#7668=DIRECTION('ref_axis',(0.499999999999998,0.86602540378444,0.));
#7669=DIRECTION('',(0.499999999999998,0.86602540378444,-1.09179756551548E-19));
#7670=DIRECTION('',(0.,0.,-1.));
#7671=DIRECTION('',(0.499999999999998,0.86602540378444,0.));
#7672=DIRECTION('center_axis',(-0.86602540378444,-0.499999999999998,0.));
#7673=DIRECTION('ref_axis',(-0.499999999999998,0.86602540378444,0.));
#7674=DIRECTION('',(-0.499999999999998,0.86602540378444,-1.09179756551649E-19));
#7675=DIRECTION('',(0.,0.,-1.));
#7676=DIRECTION('',(-0.499999999999998,0.86602540378444,0.));
#7677=DIRECTION('center_axis',(-1.60246890531963E-16,-1.,0.));
#7678=DIRECTION('ref_axis',(-1.,1.60246890531963E-16,0.));
#7679=DIRECTION('',(-1.,1.60246890531963E-16,-1.01358952973624E-31));
#7680=DIRECTION('',(0.,0.,-1.));
#7681=DIRECTION('',(-1.,1.60246890531963E-16,0.));
#7682=DIRECTION('center_axis',(0.86602540378444,-0.499999999999998,0.));
#7683=DIRECTION('ref_axis',(-0.499999999999998,-0.86602540378444,0.));
#7684=DIRECTION('',(-0.499999999999998,-0.86602540378444,1.09179756551548E-19));
#7685=DIRECTION('',(-0.499999999999998,-0.86602540378444,0.));
#7686=DIRECTION('center_axis',(0.,0.,-1.));
#7687=DIRECTION('ref_axis',(-1.,0.,0.));
#7688=DIRECTION('center_axis',(0.,0.,1.));
#7689=DIRECTION('ref_axis',(1.,0.,0.));
#7690=DIRECTION('center_axis',(0.866025403784439,0.5,0.));
#7691=DIRECTION('ref_axis',(0.5,-0.866025403784439,0.));
#7692=DIRECTION('',(0.5,-0.866025403784439,1.09179756551649E-19));
#7693=DIRECTION('',(0.,0.,-1.));
#7694=DIRECTION('',(0.5,-0.866025403784439,0.));
#7695=DIRECTION('',(0.,0.,-1.));
#7696=DIRECTION('center_axis',(1.60246890531964E-16,1.,0.));
#7697=DIRECTION('ref_axis',(1.,-1.60246890531964E-16,0.));
#7698=DIRECTION('',(1.,-1.60246890531964E-16,1.01358952973624E-31));
#7699=DIRECTION('',(0.,0.,-1.));
#7700=DIRECTION('',(1.,-1.60246890531964E-16,0.));
#7701=DIRECTION('center_axis',(-0.866025403784438,0.5,0.));
#7702=DIRECTION('ref_axis',(0.5,0.866025403784438,0.));
#7703=DIRECTION('',(0.5,0.866025403784438,-1.09179756551547E-19));
#7704=DIRECTION('',(0.,0.,-1.));
#7705=DIRECTION('',(0.5,0.866025403784438,0.));
#7706=DIRECTION('center_axis',(-0.866025403784439,-0.499999999999999,0.));
#7707=DIRECTION('ref_axis',(-0.499999999999999,0.866025403784439,0.));
#7708=DIRECTION('',(-0.499999999999999,0.866025403784439,-1.09179756551649E-19));
#7709=DIRECTION('',(0.,0.,-1.));
#7710=DIRECTION('',(-0.499999999999999,0.866025403784439,0.));
#7711=DIRECTION('center_axis',(-1.60246890531964E-16,-1.,0.));
#7712=DIRECTION('ref_axis',(-1.,1.60246890531964E-16,0.));
#7713=DIRECTION('',(-1.,1.60246890531964E-16,-1.01358952973624E-31));
#7714=DIRECTION('',(0.,0.,-1.));
#7715=DIRECTION('',(-1.,1.60246890531964E-16,0.));
#7716=DIRECTION('center_axis',(0.866025403784439,-0.5,0.));
#7717=DIRECTION('ref_axis',(-0.5,-0.866025403784439,0.));
#7718=DIRECTION('',(-0.5,-0.866025403784439,1.09179756551547E-19));
#7719=DIRECTION('',(-0.5,-0.866025403784439,0.));
#7720=DIRECTION('center_axis',(0.,0.,-1.));
#7721=DIRECTION('ref_axis',(-1.,0.,0.));
#7722=DIRECTION('center_axis',(0.,0.,1.));
#7723=DIRECTION('ref_axis',(1.,0.,0.));
#7724=DIRECTION('center_axis',(0.,0.,-1.));
#7725=DIRECTION('ref_axis',(1.,0.,0.));
#7726=DIRECTION('',(0.,0.,-1.));
#7727=DIRECTION('center_axis',(0.,0.,1.));
#7728=DIRECTION('ref_axis',(1.,0.,0.));
#7729=DIRECTION('center_axis',(0.,0.,-1.));
#7730=DIRECTION('ref_axis',(1.,0.,0.));
#7731=DIRECTION('',(0.,0.,-1.));
#7732=DIRECTION('center_axis',(0.,0.,1.));
#7733=DIRECTION('ref_axis',(1.,0.,0.));
#7734=DIRECTION('center_axis',(0.,-1.,0.));
#7735=DIRECTION('ref_axis',(-1.,0.,0.));
#7736=DIRECTION('',(0.0523359562429438,0.,0.998629534754574));
#7737=DIRECTION('',(1.,0.,0.));
#7738=DIRECTION('',(-0.0523359562429438,0.,-0.998629534754574));
#7739=DIRECTION('',(1.,0.,0.));
#7740=DIRECTION('center_axis',(0.,-1.,0.));
#7741=DIRECTION('ref_axis',(-1.,0.,0.));
#7742=DIRECTION('',(0.,0.,-1.));
#7743=DIRECTION('',(1.,0.,0.));
#7744=DIRECTION('',(0.,0.,1.));
#7745=DIRECTION('',(1.,0.,0.));
#7746=DIRECTION('center_axis',(0.,-1.,0.));
#7747=DIRECTION('ref_axis',(-1.,0.,0.));
#7748=DIRECTION('',(0.,0.,-1.));
#7749=DIRECTION('',(1.,0.,0.));
#7750=DIRECTION('',(0.,0.,1.));
#7751=DIRECTION('',(1.,0.,0.));
#7752=DIRECTION('center_axis',(0.,-1.,0.));
#7753=DIRECTION('ref_axis',(-1.,0.,0.));
#7754=DIRECTION('',(0.,0.,-1.));
#7755=DIRECTION('',(1.,0.,0.));
#7756=DIRECTION('',(0.,0.,1.));
#7757=DIRECTION('',(1.,0.,0.));
#7758=DIRECTION('center_axis',(0.,1.,0.));
#7759=DIRECTION('ref_axis',(1.,0.,0.));
#7760=DIRECTION('',(-0.0523359562429438,0.,-0.998629534754574));
#7761=DIRECTION('',(-1.,0.,0.));
#7762=DIRECTION('',(0.0523359562429438,0.,0.998629534754574));
#7763=DIRECTION('',(-1.,0.,0.));
#7764=DIRECTION('center_axis',(0.,1.,0.));
#7765=DIRECTION('ref_axis',(1.,0.,0.));
#7766=DIRECTION('',(0.,0.,1.));
#7767=DIRECTION('',(-1.,0.,0.));
#7768=DIRECTION('',(0.,0.,-1.));
#7769=DIRECTION('',(-1.,0.,0.));
#7770=DIRECTION('center_axis',(0.,1.,0.));
#7771=DIRECTION('ref_axis',(1.,0.,0.));
#7772=DIRECTION('',(0.,0.,1.));
#7773=DIRECTION('',(-1.,0.,0.));
#7774=DIRECTION('',(0.,0.,-1.));
#7775=DIRECTION('',(-1.,0.,0.));
#7776=DIRECTION('center_axis',(0.,0.,1.));
#7777=DIRECTION('ref_axis',(1.,0.,0.));
#7778=DIRECTION('center_axis',(0.,0.,1.));
#7779=DIRECTION('ref_axis',(1.,0.,0.));
#7780=DIRECTION('center_axis',(0.,0.,1.));
#7781=DIRECTION('ref_axis',(1.,0.,0.));
#7782=DIRECTION('center_axis',(0.,0.,1.));
#7783=DIRECTION('ref_axis',(1.,0.,0.));
#7784=DIRECTION('center_axis',(0.,0.,1.));
#7785=DIRECTION('ref_axis',(1.,0.,0.));
#7786=DIRECTION('',(0.,1.,0.));
#7787=DIRECTION('',(0.,-1.,0.));
#7788=DIRECTION('center_axis',(0.,0.,1.));
#7789=DIRECTION('ref_axis',(1.,0.,0.));
#7790=DIRECTION('',(0.,-1.,0.));
#7791=DIRECTION('',(0.,1.,0.));
#7792=DIRECTION('center_axis',(0.,0.,1.));
#7793=DIRECTION('ref_axis',(1.,0.,0.));
#7794=DIRECTION('',(0.,-1.,0.));
#7795=DIRECTION('',(0.,1.,0.));
#7796=DIRECTION('center_axis',(0.,0.,1.));
#7797=DIRECTION('ref_axis',(1.,0.,0.));
#7798=DIRECTION('',(0.,-1.,0.));
#7799=DIRECTION('',(-1.,0.,0.));
#7800=DIRECTION('',(0.,1.,0.));
#7801=DIRECTION('center_axis',(0.,1.,0.));
#7802=DIRECTION('ref_axis',(1.,0.,0.));
#7803=DIRECTION('',(0.,0.,1.));
#7804=DIRECTION('',(-1.,0.,0.));
#7805=DIRECTION('',(0.,0.,-1.));
#7806=DIRECTION('center_axis',(-1.,0.,0.));
#7807=DIRECTION('ref_axis',(0.,-1.,0.));
#7808=DIRECTION('',(0.,-1.,0.));
#7809=DIRECTION('',(0.,-1.,1.26069923670246E-19));
#7810=DIRECTION('center_axis',(1.,0.,0.));
#7811=DIRECTION('ref_axis',(0.,1.,0.));
#7812=DIRECTION('',(0.,1.,0.));
#7813=DIRECTION('',(0.,1.,-1.26069923670246E-19));
#7814=DIRECTION('',(0.,1.,0.));
#7815=DIRECTION('center_axis',(1.,0.,0.));
#7816=DIRECTION('ref_axis',(0.,1.,0.));
#7817=DIRECTION('',(0.,1.,0.));
#7818=DIRECTION('',(0.,1.,-1.26069923670246E-19));
#7819=DIRECTION('',(0.,1.,0.));
#7820=DIRECTION('center_axis',(1.,0.,0.));
#7821=DIRECTION('ref_axis',(0.,1.,0.));
#7822=DIRECTION('',(0.,1.,0.));
#7823=DIRECTION('',(0.,1.,-1.26069923670246E-19));
#7824=DIRECTION('',(0.,1.,0.));
#7825=DIRECTION('center_axis',(0.998629534754574,0.,-0.0523359562429438));
#7826=DIRECTION('ref_axis',(-0.0523359562429438,0.,-0.998629534754574));
#7827=DIRECTION('',(0.,-1.,0.));
#7828=DIRECTION('',(6.6070447339401E-21,-1.,1.26069923670246E-19));
#7829=DIRECTION('',(0.,-1.,0.));
#7830=DIRECTION('center_axis',(0.,0.,1.));
#7831=DIRECTION('ref_axis',(1.,0.,0.));
#7832=DIRECTION('',(0.,-1.,0.));
#7833=DIRECTION('',(0.,-1.,0.));
#7834=DIRECTION('',(0.,-1.,0.));
#7835=DIRECTION('',(0.,1.,0.));
#7836=DIRECTION('',(0.,-1.,0.));
#7837=DIRECTION('',(0.,1.,0.));
#7838=DIRECTION('',(0.,-1.,0.));
#7839=DIRECTION('',(0.,-1.,0.));
#7840=DIRECTION('',(0.,-1.,0.));
#7841=DIRECTION('',(0.,1.,0.));
#7842=DIRECTION('',(0.,1.,0.));
#7843=DIRECTION('center_axis',(0.,0.,1.));
#7844=DIRECTION('ref_axis',(1.,0.,0.));
#7845=DIRECTION('center_axis',(-1.01338750660366E-31,1.26069923670246E-19,
1.));
#7846=DIRECTION('ref_axis',(1.,0.,0.));
#7847=DIRECTION('',(0.,0.,-1.));
#7848=DIRECTION('center_axis',(0.,0.,1.));
#7849=DIRECTION('ref_axis',(1.,0.,0.));
#7850=DIRECTION('center_axis',(-1.01338750660366E-31,1.26069923670246E-19,
1.));
#7851=DIRECTION('ref_axis',(1.,0.,0.));
#7852=DIRECTION('',(0.,0.,-1.));
#7853=DIRECTION('center_axis',(1.,0.,0.));
#7854=DIRECTION('ref_axis',(0.,1.,0.));
#7855=DIRECTION('',(0.,1.,-1.26069923670246E-19));
#7856=DIRECTION('center_axis',(0.995216631131787,0.0976926666577189,1.18580395612125E-14));
#7857=DIRECTION('ref_axis',(0.0975341006448478,-0.993601284365854,0.0569524970297685));
#7858=DIRECTION('center_axis',(-1.01338750660366E-31,1.26069923670246E-19,
1.));
#7859=DIRECTION('ref_axis',(1.,0.,1.01338750660366E-31));
#7860=DIRECTION('center_axis',(-1.01338750660366E-31,1.26069923670246E-19,
1.));
#7861=DIRECTION('ref_axis',(1.,0.,1.01338750660366E-31));
#7862=DIRECTION('',(-6.60704473394009E-21,-1.,1.26069923670246E-19));
#7863=DIRECTION('center_axis',(-1.,0.,0.));
#7864=DIRECTION('ref_axis',(0.,-1.,0.));
#7865=DIRECTION('',(0.,-1.,1.26069923670246E-19));
#7866=DIRECTION('center_axis',(-1.01338750660366E-31,1.26069923670246E-19,
1.));
#7867=DIRECTION('ref_axis',(1.,0.,1.01338750660366E-31));
#7868=DIRECTION('center_axis',(-1.,0.,0.));
#7869=DIRECTION('ref_axis',(0.,-1.,0.));
#7870=DIRECTION('',(0.,-1.,1.26069923670246E-19));
#7871=DIRECTION('center_axis',(-1.01338750660366E-31,1.26069923670246E-19,
1.));
#7872=DIRECTION('ref_axis',(1.,0.,1.01338750660366E-31));
#7873=DIRECTION('center_axis',(-1.,0.,0.));
#7874=DIRECTION('ref_axis',(0.,-1.,0.));
#7875=DIRECTION('',(0.,-1.,1.26069923670246E-19));
#7876=DIRECTION('center_axis',(-0.982258063247475,0.187534256031586,1.45403402392141E-15));
#7877=DIRECTION('ref_axis',(1.48029736616688E-15,0.,1.));
#7878=DIRECTION('center_axis',(-1.01338750660366E-31,1.26069923670246E-19,
1.));
#7879=DIRECTION('ref_axis',(1.,0.,1.01338750660366E-31));
#7880=DIRECTION('',(-6.6070447339401E-21,1.,-1.26069923670246E-19));
#7881=DIRECTION('center_axis',(-0.982258063247479,-0.187534256031562,9.14061384143289E-15));
#7882=DIRECTION('ref_axis',(-0.187187393251729,0.980441281772238,0.0607928680392112));
#7883=DIRECTION('center_axis',(-0.45173408531537,0.373496730537872,-0.810207694632559));
#7884=DIRECTION('ref_axis',(-0.624418441188311,0.516273298501642,0.586142893463867));
#7885=DIRECTION('center_axis',(-2.96465769266614E-15,1.,0.));
#7886=DIRECTION('ref_axis',(0.,0.,1.));
#7887=DIRECTION('center_axis',(0.0522655346583812,-0.0518587053130894,0.997285810873755));
#7888=DIRECTION('ref_axis',(-0.998629534754574,0.,0.0523359562429445));
#7889=DIRECTION('center_axis',(0.377681861983732,-0.843372107574977,0.38220400219391));
#7890=DIRECTION('ref_axis',(0.592794689304902,0.537329962094562,0.599892463836113));
#7891=DIRECTION('center_axis',(0.995216631131786,-0.0976926666577302,0.));
#7892=DIRECTION('ref_axis',(0.,0.,1.));
#7893=DIRECTION('center_axis',(-0.0522650609395843,-0.052032719242908,0.997276771780618));
#7894=DIRECTION('ref_axis',(0.0975341006448596,0.993601284365853,0.0569524970297681));
#7895=DIRECTION('center_axis',(1.55158195278682E-16,1.,-2.96059473233375E-15));
#7896=DIRECTION('ref_axis',(0.998629534754574,0.,0.0523359562429438));
#7897=DIRECTION('center_axis',(-0.45173408531537,-0.373496730537869,-0.810207694632561));
#7898=DIRECTION('ref_axis',(-0.624418441188315,-0.516273298501641,0.586142893463864));
#7899=DIRECTION('center_axis',(0.0522655346583823,0.0518587053130918,0.997285810873755));
#7900=DIRECTION('ref_axis',(-0.187187393251729,-0.980441281772238,0.0607928680392122));
#7901=DIRECTION('center_axis',(-2.71526841737693E-16,-1.,-5.18104078158406E-15));
#7902=DIRECTION('ref_axis',(-0.998629534754574,0.,0.0523359562429439));
#7903=DIRECTION('center_axis',(-6.6070447339401E-21,1.,-1.26069923670246E-19));
#7904=DIRECTION('ref_axis',(-0.688354575693753,0.,0.725374371012289));
#7905=DIRECTION('center_axis',(-0.377681861983722,-0.843372107574983,-0.382204002193908));
#7906=DIRECTION('ref_axis',(0.592794689304909,-0.537329962094554,0.599892463836112));
#7907=DIRECTION('center_axis',(-0.0522650609395818,0.0520327192429072,0.997276771780618));
#7908=DIRECTION('ref_axis',(0.998629534754574,0.,0.0523359562429431));
#7909=DIRECTION('center_axis',(2.96465769266612E-15,-1.,0.));
#7910=DIRECTION('ref_axis',(0.,0.,1.));
#7911=DIRECTION('center_axis',(-6.60704473394009E-21,-1.,1.26069923670246E-19));
#7912=DIRECTION('ref_axis',(0.688354575693758,0.,0.725374371012284));
#7913=DIRECTION('',(6.60704473394009E-21,1.,-1.26069923670246E-19));
#7914=DIRECTION('center_axis',(-0.998629534754574,0.,-0.0523359562429438));
#7915=DIRECTION('ref_axis',(-0.0523359562429438,0.,0.998629534754574));
#7916=DIRECTION('center_axis',(-0.45173408531537,0.373496730537872,-0.81020769463256));
#7917=DIRECTION('ref_axis',(-0.624418441188311,0.516273298501643,0.586142893463866));
#7918=DIRECTION('center_axis',(-2.96465769266614E-15,1.,0.));
#7919=DIRECTION('ref_axis',(0.,0.,1.));
#7920=DIRECTION('center_axis',(-0.982258063247479,-0.187534256031562,9.14061384143289E-15));
#7921=DIRECTION('ref_axis',(-0.187187393251729,0.980441281772238,0.0607928680392111));
#7922=DIRECTION('center_axis',(0.0522655346583812,-0.0518587053130894,0.997285810873755));
#7923=DIRECTION('ref_axis',(-0.998629534754574,0.,0.0523359562429445));
#7924=DIRECTION('center_axis',(0.377681861983731,-0.843372107574978,0.38220400219391));
#7925=DIRECTION('ref_axis',(0.592794689304906,0.537329962094559,0.599892463836111));
#7926=DIRECTION('center_axis',(0.995216631131786,-0.0976926666577302,0.));
#7927=DIRECTION('ref_axis',(0.,0.,1.));
#7928=DIRECTION('center_axis',(1.55158195278682E-16,1.,-2.96059473233375E-15));
#7929=DIRECTION('ref_axis',(0.998629534754574,0.,0.0523359562429438));
#7930=DIRECTION('center_axis',(-0.0522650609395843,-0.052032719242908,0.997276771780618));
#7931=DIRECTION('ref_axis',(0.0975341006448596,0.993601284365853,0.0569524970297681));
#7932=DIRECTION('center_axis',(-0.45173408531537,-0.373496730537868,-0.810207694632561));
#7933=DIRECTION('ref_axis',(-0.624418441188315,-0.516273298501641,0.586142893463864));
#7934=DIRECTION('center_axis',(-0.982258063247475,0.187534256031586,1.45403402392141E-15));
#7935=DIRECTION('ref_axis',(1.48029736616688E-15,0.,1.));
#7936=DIRECTION('center_axis',(-2.71526841737693E-16,-1.,-5.18104078158406E-15));
#7937=DIRECTION('ref_axis',(-0.998629534754574,0.,0.0523359562429439));
#7938=DIRECTION('center_axis',(0.0522655346583823,0.0518587053130918,0.997285810873755));
#7939=DIRECTION('ref_axis',(-0.187187393251729,-0.980441281772238,0.0607928680392122));
#7940=DIRECTION('center_axis',(-6.6070447339401E-21,1.,-1.26069923670246E-19));
#7941=DIRECTION('ref_axis',(-0.688354575693753,0.,0.725374371012289));
#7942=DIRECTION('',(6.6070447339401E-21,-1.,1.26069923670246E-19));
#7943=DIRECTION('',(-6.6070447339401E-21,1.,-1.26069923670246E-19));
#7944=DIRECTION('center_axis',(-0.377681861983727,-0.843372107574981,-0.382204002193907));
#7945=DIRECTION('ref_axis',(0.592794689304909,-0.537329962094554,0.599892463836112));
#7946=DIRECTION('center_axis',(-0.0522650609395818,0.0520327192429072,0.997276771780618));
#7947=DIRECTION('ref_axis',(0.998629534754574,0.,0.0523359562429431));
#7948=DIRECTION('center_axis',(2.96465769266612E-15,-1.,0.));
#7949=DIRECTION('ref_axis',(0.,0.,1.));
#7950=DIRECTION('center_axis',(0.995216631131787,0.0976926666577189,1.18580395612125E-14));
#7951=DIRECTION('ref_axis',(0.0975341006448478,-0.993601284365854,0.0569524970297685));
#7952=DIRECTION('center_axis',(-6.60704473394009E-21,-1.,1.26069923670246E-19));
#7953=DIRECTION('ref_axis',(0.688354575693758,0.,0.725374371012284));
#7954=DIRECTION('',(6.60704473394009E-21,1.,-1.26069923670246E-19));
#7955=DIRECTION('',(-6.60704473394009E-21,-1.,1.26069923670246E-19));
#7956=DIRECTION('center_axis',(0.998629534754574,0.,-0.0523359562429438));
#7957=DIRECTION('ref_axis',(-0.0523359562429438,0.,-0.998629534754574));
#7958=DIRECTION('center_axis',(-1.01338750660366E-31,1.26069923670246E-19,
1.));
#7959=DIRECTION('ref_axis',(1.,0.,1.01338750660366E-31));
#7960=DIRECTION('center_axis',(-0.998629534754574,0.,-0.0523359562429438));
#7961=DIRECTION('ref_axis',(-0.0523359562429438,0.,0.998629534754574));
#7962=DIRECTION('axis',(0.,0.,1.));
#7963=DIRECTION('refdir',(1.,0.,0.));
#7964=DIRECTION('center_axis',(0.,0.,-1.));
#7965=DIRECTION('ref_axis',(1.,0.,0.));
#7966=DIRECTION('center_axis',(-2.77374560774598E-32,-4.07593403759339E-32,
-1.));
#7967=DIRECTION('ref_axis',(1.,0.,0.));
#7968=DIRECTION('',(0.,0.,-1.));
#7969=DIRECTION('center_axis',(-3.68477953769876E-32,1.85992248306542E-19,
1.));
#7970=DIRECTION('ref_axis',(1.,0.,0.));
#7971=DIRECTION('center_axis',(0.,0.,-1.));
#7972=DIRECTION('ref_axis',(1.,0.,0.));
#7973=DIRECTION('center_axis',(-2.77374560774598E-32,-4.07593403759339E-32,
-1.));
#7974=DIRECTION('ref_axis',(1.,0.,0.));
#7975=DIRECTION('',(0.,0.,-1.));
#7976=DIRECTION('center_axis',(-3.68477953769876E-32,1.85992248306542E-19,
1.));
#7977=DIRECTION('ref_axis',(1.,0.,0.));
#7978=DIRECTION('center_axis',(0.,0.,1.));
#7979=DIRECTION('ref_axis',(1.,0.,0.));
#7980=DIRECTION('center_axis',(0.,0.,1.));
#7981=DIRECTION('ref_axis',(1.,0.,0.));
#7982=DIRECTION('center_axis',(0.,0.,-1.));
#7983=DIRECTION('ref_axis',(1.,0.,0.));
#7984=DIRECTION('center_axis',(0.,0.,-1.));
#7985=DIRECTION('ref_axis',(1.,0.,0.));
#7986=DIRECTION('center_axis',(0.,0.,-1.));
#7987=DIRECTION('ref_axis',(1.,0.,0.));
#7988=DIRECTION('',(0.,0.,1.));
#7989=DIRECTION('center_axis',(0.,0.,1.));
#7990=DIRECTION('ref_axis',(1.,0.,0.));
#7991=DIRECTION('center_axis',(0.,0.,1.));
#7992=DIRECTION('ref_axis',(1.,0.,0.));
#7993=DIRECTION('center_axis',(0.,0.,1.));
#7994=DIRECTION('ref_axis',(1.,0.,0.));
#7995=DIRECTION('center_axis',(0.,0.,-1.));
#7996=DIRECTION('ref_axis',(1.,0.,0.));
#7997=DIRECTION('center_axis',(0.,0.,-1.));
#7998=DIRECTION('ref_axis',(1.,0.,0.));
#7999=DIRECTION('center_axis',(0.,0.,-1.));
#8000=DIRECTION('ref_axis',(1.,0.,0.));
#8001=DIRECTION('',(0.,0.,1.));
#8002=DIRECTION('center_axis',(0.,0.,1.));
#8003=DIRECTION('ref_axis',(1.,0.,0.));
#8004=DIRECTION('center_axis',(0.,0.,1.));
#8005=DIRECTION('ref_axis',(1.,0.,0.));
#8006=DIRECTION('center_axis',(0.,0.,1.));
#8007=DIRECTION('ref_axis',(1.,0.,0.));
#8008=DIRECTION('center_axis',(0.,0.,-1.));
#8009=DIRECTION('ref_axis',(1.,0.,0.));
#8010=DIRECTION('center_axis',(0.,0.,-1.));
#8011=DIRECTION('ref_axis',(1.,0.,0.));
#8012=DIRECTION('center_axis',(0.,0.,-1.));
#8013=DIRECTION('ref_axis',(1.,0.,0.));
#8014=DIRECTION('',(0.,0.,1.));
#8015=DIRECTION('center_axis',(0.,0.,1.));
#8016=DIRECTION('ref_axis',(1.,0.,0.));
#8017=DIRECTION('center_axis',(0.,0.,1.));
#8018=DIRECTION('ref_axis',(1.,0.,0.));
#8019=DIRECTION('center_axis',(0.,0.,1.));
#8020=DIRECTION('ref_axis',(1.,0.,0.));
#8021=DIRECTION('center_axis',(0.,0.,-1.));
#8022=DIRECTION('ref_axis',(1.,0.,0.));
#8023=DIRECTION('center_axis',(0.,0.,-1.));
#8024=DIRECTION('ref_axis',(1.,0.,0.));
#8025=DIRECTION('center_axis',(0.,0.,-1.));
#8026=DIRECTION('ref_axis',(1.,0.,0.));
#8027=DIRECTION('',(0.,0.,1.));
#8028=DIRECTION('center_axis',(0.,0.,1.));
#8029=DIRECTION('ref_axis',(1.,0.,0.));
#8030=DIRECTION('center_axis',(0.,0.,-1.));
#8031=DIRECTION('ref_axis',(1.,0.,0.));
#8032=DIRECTION('',(0.,0.,1.));
#8033=DIRECTION('center_axis',(-3.68477953769876E-32,1.85992248306542E-19,
1.));
#8034=DIRECTION('ref_axis',(1.,0.,0.));
#8035=DIRECTION('center_axis',(0.,0.,-1.));
#8036=DIRECTION('ref_axis',(1.,0.,0.));
#8037=DIRECTION('',(0.,0.,1.));
#8038=DIRECTION('center_axis',(-3.68477953769876E-32,1.85992248306542E-19,
1.));
#8039=DIRECTION('ref_axis',(1.,0.,0.));
#8040=DIRECTION('center_axis',(0.,0.,-1.));
#8041=DIRECTION('ref_axis',(1.,0.,0.));
#8042=DIRECTION('',(0.,0.,1.));
#8043=DIRECTION('center_axis',(-3.68477953769876E-32,1.85992248306542E-19,
1.));
#8044=DIRECTION('ref_axis',(1.,0.,0.));
#8045=DIRECTION('center_axis',(0.,0.,-1.));
#8046=DIRECTION('ref_axis',(1.,0.,0.));
#8047=DIRECTION('',(0.,0.,1.));
#8048=DIRECTION('center_axis',(-3.68477953769876E-32,1.85992248306542E-19,
1.));
#8049=DIRECTION('ref_axis',(1.,0.,0.));
#8050=DIRECTION('center_axis',(0.,1.,0.));
#8051=DIRECTION('ref_axis',(0.,0.,1.));
#8052=DIRECTION('center_axis',(0.994535543241646,-0.104398530780106,0.));
#8053=DIRECTION('ref_axis',(0.104226596285684,0.992897637377125,0.0573680949450512));
#8054=DIRECTION('center_axis',(-2.13610651414414E-33,-1.,4.07593403759339E-32));
#8055=DIRECTION('ref_axis',(0.688354575693766,0.,0.725374371012276));
#8056=DIRECTION('center_axis',(0.,1.,0.));
#8057=DIRECTION('ref_axis',(0.,0.,1.));
#8058=DIRECTION('',(2.13610651414414E-33,1.,-4.07593403759339E-32));
#8059=DIRECTION('',(-2.13610651414414E-33,-1.,4.07593403759339E-32));
#8060=DIRECTION('center_axis',(0.994535543241646,0.104398530780106,0.));
#8061=DIRECTION('ref_axis',(0.,0.,1.));
#8062=DIRECTION('center_axis',(0.979252793246429,-0.20264246079997,0.));
#8063=DIRECTION('ref_axis',(0.,0.,1.));
#8064=DIRECTION('center_axis',(0.,-1.,0.));
#8065=DIRECTION('ref_axis',(-2.77555756156289E-15,0.,1.));
#8066=DIRECTION('center_axis',(-2.13610651414429E-33,1.,-4.07593403759339E-32));
#8067=DIRECTION('ref_axis',(-0.688354575693754,0.,0.725374371012288));
#8068=DIRECTION('center_axis',(0.,-1.,0.));
#8069=DIRECTION('ref_axis',(0.,0.,1.));
#8070=DIRECTION('',(2.13610651414429E-33,-1.,4.07593403759339E-32));
#8071=DIRECTION('',(-2.13610651414429E-33,1.,-4.07593403759339E-32));
#8072=DIRECTION('center_axis',(-0.979252793246429,-0.20264246079997,-4.07695874246507E-15));
#8073=DIRECTION('ref_axis',(-4.16333634234434E-15,0.,1.));
#8074=DIRECTION('center_axis',(0.998629534754574,0.,-0.0523359562429439));
#8075=DIRECTION('ref_axis',(-0.0523359562429439,0.,-0.998629534754574));
#8076=DIRECTION('',(0.,1.,0.));
#8077=DIRECTION('center_axis',(2.77374560774598E-32,4.07593403759339E-32,
1.));
#8078=DIRECTION('ref_axis',(1.,0.,-2.77374560774598E-32));
#8079=DIRECTION('center_axis',(-0.998629534754574,0.,-0.0523359562429402));
#8080=DIRECTION('ref_axis',(-0.0523359562429402,0.,0.998629534754574));
#8081=DIRECTION('',(0.,-1.,0.));
#8082=DIRECTION('center_axis',(-3.68477953769876E-32,1.85992248306542E-19,
1.));
#8083=DIRECTION('ref_axis',(1.,0.,3.68477953769876E-32));
#8084=DIRECTION('axis',(0.,0.,1.));
#8085=DIRECTION('refdir',(1.,0.,0.));
#8086=DIRECTION('center_axis',(0.,0.,1.));
#8087=DIRECTION('ref_axis',(1.,0.,0.));
#8088=DIRECTION('',(0.,0.,-1.));
#8089=DIRECTION('center_axis',(0.,0.,-1.));
#8090=DIRECTION('ref_axis',(1.,0.,0.));
#8091=DIRECTION('center_axis',(0.,0.,1.));
#8092=DIRECTION('ref_axis',(1.,0.,0.));
#8093=DIRECTION('',(0.,0.,-1.));
#8094=DIRECTION('center_axis',(0.,0.,1.));
#8095=DIRECTION('ref_axis',(1.,0.,0.));
#8096=DIRECTION('',(0.,0.,-1.));
#8097=DIRECTION('center_axis',(0.,0.,1.));
#8098=DIRECTION('ref_axis',(1.,0.,0.));
#8099=DIRECTION('',(0.,0.,-1.));
#8100=DIRECTION('center_axis',(0.,0.,1.));
#8101=DIRECTION('ref_axis',(1.,0.,0.));
#8102=DIRECTION('',(0.,0.,-1.));
#8103=DIRECTION('center_axis',(0.,0.,1.));
#8104=DIRECTION('ref_axis',(1.,0.,0.));
#8105=DIRECTION('',(0.,0.,-1.));
#8106=DIRECTION('center_axis',(0.,0.,1.));
#8107=DIRECTION('ref_axis',(1.,0.,0.));
#8108=DIRECTION('',(0.,0.,-1.));
#8109=DIRECTION('center_axis',(0.,0.,1.));
#8110=DIRECTION('ref_axis',(1.,0.,0.));
#8111=DIRECTION('',(0.,0.,-1.));
#8112=DIRECTION('center_axis',(0.,0.,1.));
#8113=DIRECTION('ref_axis',(1.,0.,0.));
#8114=DIRECTION('',(0.,0.,-1.));
#8115=DIRECTION('center_axis',(0.,0.,1.));
#8116=DIRECTION('ref_axis',(1.,0.,0.));
#8117=DIRECTION('',(0.,0.,-1.));
#8118=DIRECTION('center_axis',(0.,0.,1.));
#8119=DIRECTION('ref_axis',(1.,0.,0.));
#8120=DIRECTION('',(0.,0.,-1.));
#8121=DIRECTION('center_axis',(0.,0.,1.));
#8122=DIRECTION('ref_axis',(1.,0.,0.));
#8123=DIRECTION('',(0.,0.,-1.));
#8124=DIRECTION('center_axis',(0.,0.,1.));
#8125=DIRECTION('ref_axis',(1.,0.,0.));
#8126=DIRECTION('',(0.,0.,-1.));
#8127=DIRECTION('center_axis',(0.,0.,1.));
#8128=DIRECTION('ref_axis',(1.,0.,0.));
#8129=DIRECTION('',(0.,0.,-1.));
#8130=DIRECTION('center_axis',(0.,0.,1.));
#8131=DIRECTION('ref_axis',(1.,0.,0.));
#8132=DIRECTION('',(0.,0.,-1.));
#8133=DIRECTION('center_axis',(0.,0.,1.));
#8134=DIRECTION('ref_axis',(1.,0.,0.));
#8135=DIRECTION('',(0.,0.,-1.));
#8136=DIRECTION('center_axis',(0.,0.,1.));
#8137=DIRECTION('ref_axis',(1.,0.,0.));
#8138=DIRECTION('',(0.,0.,-1.));
#8139=DIRECTION('center_axis',(0.,0.,1.));
#8140=DIRECTION('ref_axis',(1.,0.,0.));
#8141=DIRECTION('',(0.,0.,-1.));
#8142=DIRECTION('center_axis',(0.,0.,1.));
#8143=DIRECTION('ref_axis',(1.,0.,0.));
#8144=DIRECTION('',(0.,0.,-1.));
#8145=DIRECTION('center_axis',(0.,0.,1.));
#8146=DIRECTION('ref_axis',(1.,0.,0.));
#8147=DIRECTION('',(0.,0.,-1.));
#8148=DIRECTION('center_axis',(0.,0.,1.));
#8149=DIRECTION('ref_axis',(1.,0.,0.));
#8150=DIRECTION('',(0.,0.,-1.));
#8151=DIRECTION('center_axis',(0.,0.,1.));
#8152=DIRECTION('ref_axis',(1.,0.,0.));
#8153=DIRECTION('',(0.,0.,-1.));
#8154=DIRECTION('center_axis',(0.,0.,1.));
#8155=DIRECTION('ref_axis',(1.,0.,0.));
#8156=DIRECTION('',(0.,0.,-1.));
#8157=DIRECTION('center_axis',(0.,0.,1.));
#8158=DIRECTION('ref_axis',(1.,0.,0.));
#8159=DIRECTION('',(0.,0.,-1.));
#8160=DIRECTION('center_axis',(0.,0.,1.));
#8161=DIRECTION('ref_axis',(1.,0.,0.));
#8162=DIRECTION('',(0.,0.,-1.));
#8163=DIRECTION('center_axis',(0.,0.,1.));
#8164=DIRECTION('ref_axis',(1.,0.,0.));
#8165=DIRECTION('',(0.,0.,-1.));
#8166=DIRECTION('center_axis',(0.,0.,1.));
#8167=DIRECTION('ref_axis',(1.,0.,0.));
#8168=DIRECTION('',(0.,0.,-1.));
#8169=DIRECTION('center_axis',(0.,0.,1.));
#8170=DIRECTION('ref_axis',(1.,0.,0.));
#8171=DIRECTION('',(0.,0.,-1.));
#8172=DIRECTION('center_axis',(0.,0.,1.));
#8173=DIRECTION('ref_axis',(1.,0.,0.));
#8174=DIRECTION('',(0.,0.,-1.));
#8175=DIRECTION('center_axis',(0.,0.,1.));
#8176=DIRECTION('ref_axis',(1.,0.,0.));
#8177=DIRECTION('',(0.,0.,-1.));
#8178=DIRECTION('center_axis',(0.,0.,1.));
#8179=DIRECTION('ref_axis',(1.,-2.42503376499884E-13,0.));
#8180=DIRECTION('',(0.,0.,1.));
#8181=DIRECTION('center_axis',(0.,0.,-1.));
#8182=DIRECTION('ref_axis',(1.,-2.42503376499884E-13,0.));
#8183=DIRECTION('center_axis',(0.,0.,1.));
#8184=DIRECTION('ref_axis',(1.,-2.42503376499884E-13,0.));
#8185=DIRECTION('',(0.,0.,1.));
#8186=DIRECTION('center_axis',(0.,0.,1.));
#8187=DIRECTION('ref_axis',(1.,-2.42503376499884E-13,0.));
#8188=DIRECTION('',(0.,0.,1.));
#8189=DIRECTION('center_axis',(0.,0.,1.));
#8190=DIRECTION('ref_axis',(1.,-2.42503376499884E-13,0.));
#8191=DIRECTION('',(0.,0.,1.));
#8192=DIRECTION('center_axis',(0.,0.,1.));
#8193=DIRECTION('ref_axis',(1.,-2.42503376499884E-13,0.));
#8194=DIRECTION('',(0.,0.,1.));
#8195=DIRECTION('center_axis',(0.,0.,1.));
#8196=DIRECTION('ref_axis',(1.,-2.42503376499884E-13,0.));
#8197=DIRECTION('',(0.,0.,1.));
#8198=DIRECTION('center_axis',(0.,0.,1.));
#8199=DIRECTION('ref_axis',(1.,-2.42503376499884E-13,0.));
#8200=DIRECTION('',(0.,0.,1.));
#8201=DIRECTION('center_axis',(0.,0.,1.));
#8202=DIRECTION('ref_axis',(1.,-2.42503376499884E-13,0.));
#8203=DIRECTION('',(0.,0.,1.));
#8204=DIRECTION('center_axis',(0.,0.,1.));
#8205=DIRECTION('ref_axis',(1.,-2.42503376499884E-13,0.));
#8206=DIRECTION('',(0.,0.,1.));
#8207=DIRECTION('center_axis',(0.,0.,1.));
#8208=DIRECTION('ref_axis',(1.,-2.42503376499884E-13,0.));
#8209=DIRECTION('',(0.,0.,1.));
#8210=DIRECTION('center_axis',(0.,0.,1.));
#8211=DIRECTION('ref_axis',(1.,-2.42503376499884E-13,0.));
#8212=DIRECTION('',(0.,0.,1.));
#8213=DIRECTION('center_axis',(0.,0.,1.));
#8214=DIRECTION('ref_axis',(1.,-2.42503376499884E-13,0.));
#8215=DIRECTION('',(0.,0.,1.));
#8216=DIRECTION('center_axis',(0.,0.,1.));
#8217=DIRECTION('ref_axis',(1.,-2.42503376499884E-13,0.));
#8218=DIRECTION('',(0.,0.,1.));
#8219=DIRECTION('center_axis',(0.,0.,1.));
#8220=DIRECTION('ref_axis',(1.,-2.42503376499884E-13,0.));
#8221=DIRECTION('',(0.,0.,1.));
#8222=DIRECTION('center_axis',(0.,0.,1.));
#8223=DIRECTION('ref_axis',(1.,-2.42503376499884E-13,0.));
#8224=DIRECTION('',(0.,0.,1.));
#8225=DIRECTION('center_axis',(0.,0.,1.));
#8226=DIRECTION('ref_axis',(1.,-2.42503376499884E-13,0.));
#8227=DIRECTION('',(0.,0.,1.));
#8228=DIRECTION('center_axis',(0.,0.,1.));
#8229=DIRECTION('ref_axis',(1.,-2.42503376499884E-13,0.));
#8230=DIRECTION('',(0.,0.,1.));
#8231=DIRECTION('center_axis',(0.,0.,1.));
#8232=DIRECTION('ref_axis',(1.,-2.42503376499884E-13,0.));
#8233=DIRECTION('',(0.,0.,1.));
#8234=DIRECTION('center_axis',(0.,0.,1.));
#8235=DIRECTION('ref_axis',(1.,-2.42503376499884E-13,0.));
#8236=DIRECTION('',(0.,0.,1.));
#8237=DIRECTION('center_axis',(0.,0.,1.));
#8238=DIRECTION('ref_axis',(1.,-2.42503376499884E-13,0.));
#8239=DIRECTION('',(0.,0.,1.));
#8240=DIRECTION('center_axis',(0.,0.,1.));
#8241=DIRECTION('ref_axis',(1.,-2.42503376499884E-13,0.));
#8242=DIRECTION('',(0.,0.,1.));
#8243=DIRECTION('center_axis',(0.,0.,1.));
#8244=DIRECTION('ref_axis',(1.,-2.42503376499884E-13,0.));
#8245=DIRECTION('',(0.,0.,1.));
#8246=DIRECTION('center_axis',(0.,0.,1.));
#8247=DIRECTION('ref_axis',(1.,-2.42503376499884E-13,0.));
#8248=DIRECTION('',(0.,0.,1.));
#8249=DIRECTION('center_axis',(0.,0.,1.));
#8250=DIRECTION('ref_axis',(1.,-2.42503376499884E-13,0.));
#8251=DIRECTION('',(0.,0.,1.));
#8252=DIRECTION('center_axis',(0.,0.,1.));
#8253=DIRECTION('ref_axis',(1.,-2.42503376499884E-13,0.));
#8254=DIRECTION('',(0.,0.,1.));
#8255=DIRECTION('center_axis',(0.,0.,1.));
#8256=DIRECTION('ref_axis',(1.,-2.42503376499884E-13,0.));
#8257=DIRECTION('',(0.,0.,1.));
#8258=DIRECTION('center_axis',(0.,0.,1.));
#8259=DIRECTION('ref_axis',(1.,-2.42503376499884E-13,0.));
#8260=DIRECTION('',(0.,0.,1.));
#8261=DIRECTION('center_axis',(0.,0.,1.));
#8262=DIRECTION('ref_axis',(1.,-2.42503376499884E-13,0.));
#8263=DIRECTION('',(0.,0.,1.));
#8264=DIRECTION('center_axis',(0.,0.,1.));
#8265=DIRECTION('ref_axis',(1.,-2.42503376499884E-13,0.));
#8266=DIRECTION('',(0.,0.,1.));
#8267=DIRECTION('center_axis',(0.,0.,1.));
#8268=DIRECTION('ref_axis',(1.,-2.42503376499884E-13,0.));
#8269=DIRECTION('',(0.,0.,1.));
#8270=DIRECTION('center_axis',(0.,0.,-1.));
#8271=DIRECTION('ref_axis',(1.,0.,0.));
#8272=DIRECTION('center_axis',(0.,0.,-1.));
#8273=DIRECTION('ref_axis',(1.,0.,0.));
#8274=DIRECTION('',(0.707106781186547,8.65956056235493E-17,0.707106781186548));
#8275=DIRECTION('center_axis',(0.,0.,1.));
#8276=DIRECTION('ref_axis',(1.,0.,0.));
#8277=DIRECTION('center_axis',(0.,0.,1.));
#8278=DIRECTION('ref_axis',(1.,-2.42503376499884E-13,0.));
#8279=DIRECTION('center_axis',(0.,0.,-1.));
#8280=DIRECTION('ref_axis',(1.,-2.42503376499884E-13,0.));
#8281=DIRECTION('center_axis',(0.,0.,1.));
#8282=DIRECTION('ref_axis',(1.,0.,0.));
#8283=DIRECTION('center_axis',(-1.92296268638356E-16,-1.,0.));
#8284=DIRECTION('ref_axis',(1.,-1.92296268638356E-16,0.));
#8285=DIRECTION('',(1.,-1.92296268638356E-16,0.));
#8286=DIRECTION('',(0.,0.,1.));
#8287=DIRECTION('',(1.,-1.92296268638356E-16,0.));
#8288=DIRECTION('',(0.,0.,1.));
#8289=DIRECTION('center_axis',(-0.866025403784439,-0.5,0.));
#8290=DIRECTION('ref_axis',(0.5,-0.866025403784439,0.));
#8291=DIRECTION('',(0.5,-0.866025403784439,0.));
#8292=DIRECTION('',(0.,0.,1.));
#8293=DIRECTION('',(0.5,-0.866025403784439,0.));
#8294=DIRECTION('center_axis',(-0.866025403784439,0.5,0.));
#8295=DIRECTION('ref_axis',(-0.5,-0.866025403784439,0.));
#8296=DIRECTION('',(-0.5,-0.866025403784439,0.));
#8297=DIRECTION('',(0.,0.,1.));
#8298=DIRECTION('',(-0.5,-0.866025403784438,0.));
#8299=DIRECTION('center_axis',(1.92296268638356E-16,1.,0.));
#8300=DIRECTION('ref_axis',(-1.,1.92296268638356E-16,0.));
#8301=DIRECTION('',(-1.,1.92296268638356E-16,0.));
#8302=DIRECTION('',(0.,0.,1.));
#8303=DIRECTION('',(-1.,1.92296268638356E-16,0.));
#8304=DIRECTION('center_axis',(0.866025403784439,0.5,0.));
#8305=DIRECTION('ref_axis',(-0.5,0.866025403784439,0.));
#8306=DIRECTION('',(-0.5,0.866025403784439,0.));
#8307=DIRECTION('',(0.,0.,1.));
#8308=DIRECTION('',(-0.5,0.866025403784439,0.));
#8309=DIRECTION('center_axis',(0.866025403784439,-0.5,0.));
#8310=DIRECTION('ref_axis',(0.5,0.866025403784439,0.));
#8311=DIRECTION('',(0.5,0.866025403784439,0.));
#8312=DIRECTION('',(0.5,0.866025403784439,0.));
#8313=DIRECTION('center_axis',(0.,0.,1.));
#8314=DIRECTION('ref_axis',(1.,0.,0.));
#8315=DIRECTION('center_axis',(0.,0.,1.));
#8316=DIRECTION('ref_axis',(1.,0.,0.));
#8317=DIRECTION('center_axis',(0.,0.,1.));
#8318=DIRECTION('ref_axis',(1.,0.,0.));
#8319=DIRECTION('center_axis',(0.,0.,1.));
#8320=DIRECTION('ref_axis',(1.,0.,0.));
#8321=DIRECTION('',(0.,0.,-1.));
#8322=DIRECTION('center_axis',(0.,0.,1.));
#8323=DIRECTION('ref_axis',(1.,0.,0.));
#8324=DIRECTION('center_axis',(0.,0.,1.));
#8325=DIRECTION('ref_axis',(1.,0.,0.));
#8326=DIRECTION('center_axis',(0.,0.,1.));
#8327=DIRECTION('ref_axis',(1.,0.,0.));
#8328=DIRECTION('axis',(0.,0.,1.));
#8329=DIRECTION('refdir',(1.,0.,0.));
#8330=DIRECTION('center_axis',(0.,0.,-1.));
#8331=DIRECTION('ref_axis',(1.,0.,0.));
#8332=DIRECTION('',(0.,0.,-1.));
#8333=DIRECTION('center_axis',(0.,0.,-1.));
#8334=DIRECTION('ref_axis',(1.,0.,0.));
#8335=DIRECTION('center_axis',(0.,0.,-1.));
#8336=DIRECTION('ref_axis',(1.,0.,0.));
#8337=DIRECTION('',(0.,0.,-1.));
#8338=DIRECTION('center_axis',(0.,0.,-1.));
#8339=DIRECTION('ref_axis',(1.,0.,0.));
#8340=DIRECTION('center_axis',(0.,0.,-1.));
#8341=DIRECTION('ref_axis',(1.,0.,0.));
#8342=DIRECTION('',(0.,0.,-1.));
#8343=DIRECTION('center_axis',(0.,0.,-1.));
#8344=DIRECTION('ref_axis',(1.,0.,0.));
#8345=DIRECTION('',(0.,0.,-1.));
#8346=DIRECTION('center_axis',(0.,0.,-1.));
#8347=DIRECTION('ref_axis',(0.937385399639056,-0.348293859468591,0.));
#8348=DIRECTION('',(0.,0.,-1.));
#8349=DIRECTION('center_axis',(0.,0.,-1.));
#8350=DIRECTION('ref_axis',(1.,0.,0.));
#8351=DIRECTION('center_axis',(0.,0.,-1.));
#8352=DIRECTION('ref_axis',(0.28361887368566,0.958937085782627,0.));
#8353=DIRECTION('',(1.22464679914735E-16,8.07419868282478E-31,-1.));
#8354=DIRECTION('center_axis',(0.,0.,1.));
#8355=DIRECTION('ref_axis',(1.,6.71554824363804E-15,0.));
#8356=DIRECTION('center_axis',(0.,0.,-1.));
#8357=DIRECTION('ref_axis',(1.,6.71554824363804E-15,0.));
#8358=DIRECTION('',(1.22464679914735E-16,8.07419868282478E-31,-1.));
#8359=DIRECTION('center_axis',(0.,0.,-1.));
#8360=DIRECTION('ref_axis',(1.,6.71554824363804E-15,0.));
#8361=DIRECTION('',(1.22464679914735E-16,8.07419868282478E-31,-1.));
#8362=DIRECTION('center_axis',(0.,0.,-1.));
#8363=DIRECTION('ref_axis',(1.,6.71554824363804E-15,0.));
#8364=DIRECTION('',(1.22464679914735E-16,8.07419868282478E-31,-1.));
#8365=DIRECTION('center_axis',(0.,0.,-1.));
#8366=DIRECTION('ref_axis',(-0.60895050335979,-0.793208222636313,0.));
#8367=DIRECTION('',(1.22464679914735E-16,8.07419868282478E-31,-1.));
#8368=DIRECTION('center_axis',(0.,0.,-1.));
#8369=DIRECTION('ref_axis',(1.,6.71554824363804E-15,0.));
#8370=DIRECTION('center_axis',(0.,0.,-1.));
#8371=DIRECTION('ref_axis',(1.,6.71554824363804E-15,0.));
#8372=DIRECTION('center_axis',(0.,0.,1.));
#8373=DIRECTION('ref_axis',(1.,0.,0.));
#8374=DIRECTION('',(0.5,0.866025403784439,0.));
#8375=DIRECTION('',(-0.5,0.866025403784439,0.));
#8376=DIRECTION('',(-1.,0.,0.));
#8377=DIRECTION('',(-0.5,-0.866025403784439,0.));
#8378=DIRECTION('',(0.5,-0.866025403784439,0.));
#8379=DIRECTION('',(1.,-3.49629579342466E-16,0.));
#8380=DIRECTION('center_axis',(0.,0.,-1.));
#8381=DIRECTION('ref_axis',(1.,0.,0.));
#8382=DIRECTION('center_axis',(-3.49629579342466E-16,-1.,0.));
#8383=DIRECTION('ref_axis',(1.,-3.49629579342466E-16,0.));
#8384=DIRECTION('',(1.,-3.49629579342466E-16,0.));
#8385=DIRECTION('',(0.,0.,1.));
#8386=DIRECTION('',(0.,0.,1.));
#8387=DIRECTION('center_axis',(-0.866025403784439,-0.5,0.));
#8388=DIRECTION('ref_axis',(0.5,-0.866025403784439,0.));
#8389=DIRECTION('',(0.5,-0.866025403784439,0.));
#8390=DIRECTION('',(0.,0.,1.));
#8391=DIRECTION('center_axis',(-0.866025403784439,0.5,0.));
#8392=DIRECTION('ref_axis',(-0.5,-0.866025403784439,0.));
#8393=DIRECTION('',(-0.5,-0.866025403784439,0.));
#8394=DIRECTION('',(0.,0.,1.));
#8395=DIRECTION('center_axis',(0.,1.,0.));
#8396=DIRECTION('ref_axis',(-1.,0.,0.));
#8397=DIRECTION('',(-1.,0.,0.));
#8398=DIRECTION('',(0.,0.,1.));
#8399=DIRECTION('center_axis',(0.866025403784439,0.5,0.));
#8400=DIRECTION('ref_axis',(-0.5,0.866025403784439,0.));
#8401=DIRECTION('',(-0.5,0.866025403784439,0.));
#8402=DIRECTION('',(0.,0.,1.));
#8403=DIRECTION('center_axis',(0.866025403784439,-0.5,0.));
#8404=DIRECTION('ref_axis',(0.5,0.866025403784439,0.));
#8405=DIRECTION('',(0.5,0.866025403784439,0.));
#8406=DIRECTION('center_axis',(0.,0.,1.));
#8407=DIRECTION('ref_axis',(1.,0.,0.));
#8408=DIRECTION('',(0.,0.,1.));
#8409=DIRECTION('',(1.,0.,0.));
#8410=DIRECTION('',(0.,-1.22464679914735E-16,-1.));
#8411=DIRECTION('',(1.,0.,0.));
#8412=DIRECTION('',(0.,0.,1.));
#8413=DIRECTION('',(1.,0.,0.));
#8414=DIRECTION('',(0.,-1.22464679914735E-16,-1.));
#8415=DIRECTION('',(1.,0.,0.));
#8416=DIRECTION('',(0.,0.,1.));
#8417=DIRECTION('',(1.,0.,0.));
#8418=DIRECTION('',(0.,-1.22464679914735E-16,-1.));
#8419=DIRECTION('',(1.,0.,0.));
#8420=DIRECTION('',(0.,-1.22464679914735E-16,-1.));
#8421=DIRECTION('',(1.,0.,0.));
#8422=DIRECTION('',(0.,0.,1.));
#8423=DIRECTION('',(1.,0.,0.));
#8424=DIRECTION('axis',(0.,0.,1.));
#8425=DIRECTION('refdir',(1.,0.,0.));
#8426=DIRECTION('center_axis',(0.,0.,1.));
#8427=DIRECTION('ref_axis',(1.,0.,0.));
#8428=DIRECTION('center_axis',(0.,0.,-1.));
#8429=DIRECTION('ref_axis',(1.,0.,0.));
#8430=DIRECTION('',(0.,0.,-1.));
#8431=DIRECTION('center_axis',(0.,0.,-1.));
#8432=DIRECTION('ref_axis',(1.,0.,0.));
#8433=DIRECTION('center_axis',(0.,0.,1.));
#8434=DIRECTION('ref_axis',(1.,0.,0.));
#8435=DIRECTION('center_axis',(0.,0.,1.));
#8436=DIRECTION('ref_axis',(1.,0.,0.));
#8437=DIRECTION('',(0.,0.,-1.));
#8438=DIRECTION('center_axis',(0.,0.,1.));
#8439=DIRECTION('ref_axis',(1.,0.,0.));
#8440=DIRECTION('center_axis',(0.,0.,1.));
#8441=DIRECTION('ref_axis',(1.,0.,0.));
#8442=DIRECTION('center_axis',(0.,0.,1.));
#8443=DIRECTION('ref_axis',(1.,0.,0.));
#8444=DIRECTION('',(0.,0.,1.));
#8445=DIRECTION('',(1.,0.,0.));
#8446=DIRECTION('',(0.,0.,1.));
#8447=DIRECTION('',(1.,0.,0.));
#8448=DIRECTION('',(0.,-1.22464679914735E-16,-1.));
#8449=DIRECTION('',(1.,0.,0.));
#8450=DIRECTION('',(0.,0.,1.));
#8451=DIRECTION('',(1.,0.,0.));
#8452=DIRECTION('',(0.,0.,1.));
#8453=DIRECTION('',(1.,0.,0.));
#8454=DIRECTION('',(0.,0.,1.));
#8455=DIRECTION('',(1.,0.,0.));
#8456=DIRECTION('',(0.,-1.22464679914735E-16,-1.));
#8457=DIRECTION('',(1.,0.,0.));
#8458=DIRECTION('',(0.,0.,1.));
#8459=DIRECTION('',(1.,0.,0.));
#8460=CARTESIAN_POINT('',(0.,0.,0.));
#8461=CARTESIAN_POINT('',(0.,0.,0.));
#8462=CARTESIAN_POINT('Origin',(6.,-2.5,0.3));
#8463=CARTESIAN_POINT('',(5.83,-2.5,0.6));
#8464=CARTESIAN_POINT('Origin',(6.,-2.5,0.6));
#8465=CARTESIAN_POINT('',(5.83,-2.5,0.));
#8466=CARTESIAN_POINT('',(5.83,-2.5,0.3));
#8467=CARTESIAN_POINT('Origin',(6.,-2.5,0.));
#8468=CARTESIAN_POINT('Origin',(14.,-2.5,0.3));
#8469=CARTESIAN_POINT('',(13.83,-2.5,0.6));
#8470=CARTESIAN_POINT('Origin',(14.,-2.5,0.6));
#8471=CARTESIAN_POINT('',(13.83,-2.5,0.));
#8472=CARTESIAN_POINT('',(13.83,-2.5,0.3));
#8473=CARTESIAN_POINT('Origin',(14.,-2.5,0.));
#8474=CARTESIAN_POINT('Origin',(0.,0.,0.3));
#8475=CARTESIAN_POINT('',(-0.41,5.02105187650415E-17,0.6));
#8476=CARTESIAN_POINT('Origin',(0.,0.,0.6));
#8477=CARTESIAN_POINT('',(-0.41,5.02105187650415E-17,0.));
#8478=CARTESIAN_POINT('',(-0.41,5.02105187650415E-17,0.3));
#8479=CARTESIAN_POINT('Origin',(0.,0.,0.));
#8480=CARTESIAN_POINT('Origin',(-2.29138429764753,-0.0507555356354263,0.175));
#8481=CARTESIAN_POINT('',(-2.40887839462292,0.141130204261882,0.3));
#8482=CARTESIAN_POINT('',(-2.2,-0.2,0.3));
#8483=CARTESIAN_POINT('',(-2.63798141173519,0.515290294708827,0.3));
#8484=CARTESIAN_POINT('',(-2.2,-0.2,0.));
#8485=CARTESIAN_POINT('',(-2.2,-0.199999999999998,1.9729463250961E-32));
#8486=CARTESIAN_POINT('',(-2.2,-0.2,0.));
#8487=CARTESIAN_POINT('Origin',(-4.5,3.55625,0.15));
#8488=CARTESIAN_POINT('',(-6.8,-0.2,0.));
#8489=CARTESIAN_POINT('',(-6.59112160537708,0.141130204261881,0.3));
#8490=CARTESIAN_POINT('',(-6.8,-0.200000000000001,1.9729463250961E-32));
#8491=CARTESIAN_POINT('Origin',(-4.5,3.55625,0.));
#8492=CARTESIAN_POINT('Origin',(-4.5,3.55625,0.3));
#8493=CARTESIAN_POINT('Origin',(-6.70861570235247,-0.0507555356354272,0.175));
#8494=CARTESIAN_POINT('',(-6.8,-0.2,0.3));
#8495=CARTESIAN_POINT('',(-6.3074808585895,0.604358706488338,0.3));
#8496=CARTESIAN_POINT('',(-6.8,-0.2,0.));
#8497=CARTESIAN_POINT('Origin',(-2.2,-0.2,0.));
#8498=CARTESIAN_POINT('',(-2.,0.0666666666666669,0.3));
#8499=CARTESIAN_POINT('',(-2.,0.0666666666666669,0.));
#8500=CARTESIAN_POINT('',(-2.,0.0666666666666667,0.));
#8501=CARTESIAN_POINT('',(-1.6,0.6,0.3));
#8502=CARTESIAN_POINT('',(-1.6,0.6,0.));
#8503=CARTESIAN_POINT('Origin',(-1.6,1.2,0.));
#8504=CARTESIAN_POINT('',(-2.4,1.4,0.));
#8505=CARTESIAN_POINT('',(-1.6,1.2,0.));
#8506=CARTESIAN_POINT('',(-2.4,1.4,0.));
#8507=CARTESIAN_POINT('',(-2.4,1.4,0.3));
#8508=CARTESIAN_POINT('',(-2.4,1.4,0.));
#8509=CARTESIAN_POINT('',(-1.6,1.2,0.3));
#8510=CARTESIAN_POINT('',(-2.4,1.4,0.3));
#8511=CARTESIAN_POINT('',(-1.6,1.2,0.));
#8512=CARTESIAN_POINT('Origin',(-6.8,1.38777878078145E-17,0.));
#8513=CARTESIAN_POINT('',(-6.8,0.200000000000001,0.));
#8514=CARTESIAN_POINT('Origin',(-6.8,1.38777878078145E-17,0.));
#8515=CARTESIAN_POINT('',(-6.8,0.200000000000002,0.3));
#8516=CARTESIAN_POINT('Origin',(-6.8,1.38777878078145E-17,0.3));
#8517=CARTESIAN_POINT('',(-6.8,0.200000000000001,0.));
#8518=CARTESIAN_POINT('Origin',(-1.47616279069767,-10.6540697674419,0.));
#8519=CARTESIAN_POINT('Origin',(-1.47616279069767,-10.6540697674419,0.));
#8520=CARTESIAN_POINT('Origin',(-1.47616279069767,-10.6540697674419,0.3));
#8521=CARTESIAN_POINT('Origin',(-4.3,0.275886703260749,0.3));
#8522=CARTESIAN_POINT('',(-2.,1.2,0.3));
#8523=CARTESIAN_POINT('',(-2.,0.737943351630374,0.3));
#8524=CARTESIAN_POINT('',(-2.75,1.2,0.3));
#8525=CARTESIAN_POINT('Origin',(-1.2,1.2,0.));
#8526=CARTESIAN_POINT('',(-2.,1.2,0.6));
#8527=CARTESIAN_POINT('',(-2.,1.2,0.));
#8528=CARTESIAN_POINT('',(-1.2,1.2,0.6));
#8529=CARTESIAN_POINT('',(-2.,1.2,0.6));
#8530=CARTESIAN_POINT('',(-1.2,1.2,0.));
#8531=CARTESIAN_POINT('',(-1.2,1.2,0.));
#8532=CARTESIAN_POINT('',(-2.,1.2,0.));
#8533=CARTESIAN_POINT('Origin',(-2.,1.2,0.));
#8534=CARTESIAN_POINT('',(-2.,0.,0.));
#8535=CARTESIAN_POINT('',(-2.,0.,0.));
#8536=CARTESIAN_POINT('',(-2.,0.,0.6));
#8537=CARTESIAN_POINT('',(-2.,0.,0.));
#8538=CARTESIAN_POINT('',(-2.,0.,0.6));
#8539=CARTESIAN_POINT('Origin',(-2.,0.,0.));
#8540=CARTESIAN_POINT('',(-1.4,0.,0.6));
#8541=CARTESIAN_POINT('',(-1.4,0.,0.));
#8542=CARTESIAN_POINT('',(-1.4,0.,0.));
#8543=CARTESIAN_POINT('',(-1.2,0.,0.6));
#8544=CARTESIAN_POINT('',(-1.2,0.,0.));
#8545=CARTESIAN_POINT('Origin',(-1.2,0.,0.));
#8546=CARTESIAN_POINT('',(-1.2,0.721110255092798,0.));
#8547=CARTESIAN_POINT('',(-1.2,0.721110255092798,0.6));
#8548=CARTESIAN_POINT('',(-1.2,0.721110255092798,0.));
#8549=CARTESIAN_POINT('',(-1.2,1.2,0.));
#8550=CARTESIAN_POINT('',(-1.2,1.2,0.6));
#8551=CARTESIAN_POINT('Origin',(0.,0.,0.));
#8552=CARTESIAN_POINT('',(0.533017816115691,-1.29456247732709,0.));
#8553=CARTESIAN_POINT('Origin',(0.,0.,0.));
#8554=CARTESIAN_POINT('',(0.533017816115691,-1.29456247732709,0.6));
#8555=CARTESIAN_POINT('',(0.533017816115691,-1.29456247732709,0.));
#8556=CARTESIAN_POINT('Origin',(0.,0.,0.6));
#8557=CARTESIAN_POINT('Origin',(0.,0.,0.));
#8558=CARTESIAN_POINT('',(0.993295878967653,0.986591757935306,0.6));
#8559=CARTESIAN_POINT('Origin',(0.,0.,0.6));
#8560=CARTESIAN_POINT('',(0.993295878967653,0.986591757935306,0.));
#8561=CARTESIAN_POINT('',(0.993295878967653,0.986591757935306,0.));
#8562=CARTESIAN_POINT('Origin',(0.,0.,0.));
#8563=CARTESIAN_POINT('Origin',(0.,0.,0.6));
#8564=CARTESIAN_POINT('',(0.549222100239177,-1.30351747644797,0.6));
#8565=CARTESIAN_POINT('',(0.,-1.,0.6));
#8566=CARTESIAN_POINT('',(3.51486278039743,-2.94242416811437,0.6));
#8567=CARTESIAN_POINT('Origin',(2.1,-2.,0.6));
#8568=CARTESIAN_POINT('',(3.8,-3.1,0.6));
#8569=CARTESIAN_POINT('',(0.,-1.,0.6));
#8570=CARTESIAN_POINT('',(15.2,-3.1,0.6));
#8571=CARTESIAN_POINT('',(3.8,-3.1,0.6));
#8572=CARTESIAN_POINT('',(15.2,-1.9,0.6));
#8573=CARTESIAN_POINT('',(15.2,-3.1,0.6));
#8574=CARTESIAN_POINT('',(3.8,-1.9,0.6));
#8575=CARTESIAN_POINT('',(15.2,-1.9,0.6));
#8576=CARTESIAN_POINT('',(3.79686161498349,-1.89674952980433,0.6));
#8577=CARTESIAN_POINT('',(3.8,-1.9,0.6));
#8578=CARTESIAN_POINT('',(2.26270761578574,-0.307804316349519,0.6));
#8579=CARTESIAN_POINT('Origin',(2.1,-2.,0.6));
#8580=CARTESIAN_POINT('',(1.,1.,0.6));
#8581=CARTESIAN_POINT('',(3.8,-1.9,0.6));
#8582=CARTESIAN_POINT('',(1.,1.,0.6));
#8583=CARTESIAN_POINT('',(3.3,-2.,0.6));
#8584=CARTESIAN_POINT('Origin',(2.1,-2.,0.6));
#8585=CARTESIAN_POINT('Origin',(2.1,-2.,0.1));
#8586=CARTESIAN_POINT('',(0.9,-2.,0.));
#8587=CARTESIAN_POINT('Origin',(2.1,-2.,0.));
#8588=CARTESIAN_POINT('',(1.,-2.,0.1));
#8589=CARTESIAN_POINT('Origin',(0.9,-2.,0.1));
#8590=CARTESIAN_POINT('Origin',(2.1,-2.,0.1));
#8591=CARTESIAN_POINT('Origin',(2.1,-2.,0.3));
#8592=CARTESIAN_POINT('',(3.2,-2.,0.5));
#8593=CARTESIAN_POINT('',(1.,-2.,0.5));
#8594=CARTESIAN_POINT('Origin',(2.1,-2.,0.5));
#8595=CARTESIAN_POINT('Origin',(2.1,-2.,0.5));
#8596=CARTESIAN_POINT('',(1.,-2.,0.3));
#8597=CARTESIAN_POINT('Origin',(0.,0.,0.));
#8598=CARTESIAN_POINT('',(1.,1.,0.));
#8599=CARTESIAN_POINT('',(1.,1.,0.));
#8600=CARTESIAN_POINT('',(2.26270761578574,-0.307804316349519,0.));
#8601=CARTESIAN_POINT('',(3.8,-1.9,0.));
#8602=CARTESIAN_POINT('',(3.79686161498349,-1.89674952980433,0.));
#8603=CARTESIAN_POINT('Origin',(2.1,-2.,0.));
#8604=CARTESIAN_POINT('',(3.8,-1.9,0.));
#8605=CARTESIAN_POINT('',(3.8,-1.9,0.));
#8606=CARTESIAN_POINT('',(15.2,-1.9,0.));
#8607=CARTESIAN_POINT('',(15.2,-1.9,0.));
#8608=CARTESIAN_POINT('',(15.2,-3.1,0.));
#8609=CARTESIAN_POINT('',(15.2,-3.1,0.));
#8610=CARTESIAN_POINT('',(3.8,-3.1,0.));
#8611=CARTESIAN_POINT('',(3.8,-3.1,0.));
#8612=CARTESIAN_POINT('',(3.51486278039743,-2.94242416811437,0.));
#8613=CARTESIAN_POINT('',(0.,-1.,0.));
#8614=CARTESIAN_POINT('',(0.549222100239177,-1.30351747644797,0.));
#8615=CARTESIAN_POINT('Origin',(2.1,-2.,0.));
#8616=CARTESIAN_POINT('',(0.,-1.,0.));
#8617=CARTESIAN_POINT('Origin',(2.1,-2.,0.5));
#8618=CARTESIAN_POINT('Origin',(3.3,-2.,0.5));
#8619=CARTESIAN_POINT('Origin',(2.1,-2.,0.));
#8620=CARTESIAN_POINT('',(2.26270761578574,-0.307804316349519,0.));
#8621=CARTESIAN_POINT('',(3.79686161498349,-1.89674952980433,0.));
#8622=CARTESIAN_POINT('Origin',(2.1,-2.,0.));
#8623=CARTESIAN_POINT('',(0.549222100239177,-1.30351747644797,0.));
#8624=CARTESIAN_POINT('',(3.51486278039743,-2.94242416811437,0.));
#8625=CARTESIAN_POINT('Origin',(0.,-1.,0.));
#8626=CARTESIAN_POINT('',(3.8,-3.1,0.));
#8627=CARTESIAN_POINT('Origin',(3.8,-1.9,0.));
#8628=CARTESIAN_POINT('',(3.8,-1.9,0.));
#8629=CARTESIAN_POINT('Origin',(0.,-1.,0.));
#8630=CARTESIAN_POINT('Origin',(1.,1.,0.));
#8631=CARTESIAN_POINT('',(1.,1.,0.));
#8632=CARTESIAN_POINT('Origin',(3.8,-1.9,0.));
#8633=CARTESIAN_POINT('Origin',(15.2,-1.9,0.));
#8634=CARTESIAN_POINT('',(15.2,-1.9,0.));
#8635=CARTESIAN_POINT('Origin',(15.2,-3.1,0.));
#8636=CARTESIAN_POINT('',(15.2,-3.1,0.));
#8637=CARTESIAN_POINT('Origin',(3.8,-3.1,0.));
#8638=CARTESIAN_POINT('',(0.,0.,0.));
#8639=CARTESIAN_POINT('Origin',(0.,0.,0.75));
#8640=CARTESIAN_POINT('',(-0.3,-3.67394039744206E-17,0.7));
#8641=CARTESIAN_POINT('Origin',(0.,0.,0.7));
#8642=CARTESIAN_POINT('',(-0.3,-3.67394039744206E-17,0.8));
#8643=CARTESIAN_POINT('',(-0.3,-3.67394039744206E-17,0.75));
#8644=CARTESIAN_POINT('Origin',(0.,0.,0.8));
#8645=CARTESIAN_POINT('Origin',(0.7,0.,0.7));
#8646=CARTESIAN_POINT('',(-0.4,4.89858719658941E-17,0.7));
#8647=CARTESIAN_POINT('Origin',(0.,0.,0.7));
#8648=CARTESIAN_POINT('Origin',(0.3,0.,0.8));
#8649=CARTESIAN_POINT('',(-0.4,-4.89858719658941E-17,0.8));
#8650=CARTESIAN_POINT('Origin',(0.,0.,0.8));
#8651=CARTESIAN_POINT('Origin',(0.,0.,-0.7));
#8652=CARTESIAN_POINT('',(-0.4,-4.89858719658941E-17,0.9));
#8653=CARTESIAN_POINT('Origin',(0.,0.,0.9));
#8654=CARTESIAN_POINT('',(-0.4,-4.89858719658941E-17,-0.7));
#8655=CARTESIAN_POINT('Origin',(0.,0.,-0.7));
#8656=CARTESIAN_POINT('',(-0.6,-7.34788079488412E-17,-0.7));
#8657=CARTESIAN_POINT('Origin',(0.,0.,-0.7));
#8658=CARTESIAN_POINT('',(-0.4,-4.89858719658941E-17,-0.7));
#8659=CARTESIAN_POINT('Origin',(0.,0.,-0.7));
#8660=CARTESIAN_POINT('Origin',(0.,0.,-0.8));
#8661=CARTESIAN_POINT('',(-0.6,-7.34788079488412E-17,-0.8));
#8662=CARTESIAN_POINT('',(-0.6,-7.34788079488412E-17,-0.8));
#8663=CARTESIAN_POINT('Origin',(0.,0.,-0.8));
#8664=CARTESIAN_POINT('Origin',(0.,0.,-0.8));
#8665=CARTESIAN_POINT('Origin',(0.,0.,-0.7));
#8666=CARTESIAN_POINT('',(-0.4,-4.89858719658941E-17,-0.7));
#8667=CARTESIAN_POINT('Origin',(0.,0.,0.9));
#8668=CARTESIAN_POINT('',(0.,0.,0.));
#8669=CARTESIAN_POINT('Origin',(-0.1,0.,0.1));
#8670=CARTESIAN_POINT('',(-0.1,0.282842712474619,0.));
#8671=CARTESIAN_POINT('',(-0.1,0.282842712474619,0.1));
#8672=CARTESIAN_POINT('',(-0.1,0.282842712474619,0.));
#8673=CARTESIAN_POINT('',(-0.1,0.591607978309962,0.));
#8674=CARTESIAN_POINT('',(-0.1,0.,0.));
#8675=CARTESIAN_POINT('',(-0.1,0.591607978309962,0.1));
#8676=CARTESIAN_POINT('',(-0.1,0.591607978309962,0.));
#8677=CARTESIAN_POINT('',(-0.1,0.,0.1));
#8678=CARTESIAN_POINT('Origin',(0.1,1.2,0.1));
#8679=CARTESIAN_POINT('',(0.1,0.282842712474619,0.1));
#8680=CARTESIAN_POINT('',(0.1,0.282842712474619,0.));
#8681=CARTESIAN_POINT('',(0.1,0.282842712474619,0.));
#8682=CARTESIAN_POINT('',(0.1,0.591607978309962,0.1));
#8683=CARTESIAN_POINT('',(0.1,0.6,0.1));
#8684=CARTESIAN_POINT('',(0.1,0.591607978309962,0.));
#8685=CARTESIAN_POINT('',(0.1,0.591607978309962,0.));
#8686=CARTESIAN_POINT('',(0.1,0.6,0.));
#8687=CARTESIAN_POINT('Origin',(0.,0.,0.));
#8688=CARTESIAN_POINT('Origin',(0.,0.,0.));
#8689=CARTESIAN_POINT('Origin',(0.,0.,0.));
#8690=CARTESIAN_POINT('Origin',(0.,0.,0.));
#8691=CARTESIAN_POINT('Origin',(0.,0.,0.1));
#8692=CARTESIAN_POINT('Origin',(0.,0.,0.));
#8693=CARTESIAN_POINT('Origin',(0.,0.,0.1));
#8694=CARTESIAN_POINT('Origin',(0.,0.,0.1));
#8695=CARTESIAN_POINT('',(0.,0.,0.));
#8696=CARTESIAN_POINT('',(0.,0.,0.));
#8697=CARTESIAN_POINT('Origin',(9.,-1.,0.8));
#8698=CARTESIAN_POINT('',(8.85,-1.,0.9));
#8699=CARTESIAN_POINT('Origin',(9.,-1.,0.9));
#8700=CARTESIAN_POINT('',(8.85,-1.,0.7));
#8701=CARTESIAN_POINT('',(8.85,-1.,0.8));
#8702=CARTESIAN_POINT('Origin',(9.,-1.,0.7));
#8703=CARTESIAN_POINT('Origin',(3.,-1.,0.8));
#8704=CARTESIAN_POINT('',(2.85,-1.,0.9));
#8705=CARTESIAN_POINT('Origin',(3.,-1.,0.9));
#8706=CARTESIAN_POINT('',(2.85,-1.,0.7));
#8707=CARTESIAN_POINT('',(2.85,-1.,0.8));
#8708=CARTESIAN_POINT('Origin',(3.,-1.,0.7));
#8709=CARTESIAN_POINT('Origin',(3.,1.,0.8));
#8710=CARTESIAN_POINT('',(2.85,1.,0.9));
#8711=CARTESIAN_POINT('Origin',(3.,1.,0.9));
#8712=CARTESIAN_POINT('',(2.85,1.,0.7));
#8713=CARTESIAN_POINT('',(2.85,1.,0.8));
#8714=CARTESIAN_POINT('Origin',(3.,1.,0.7));
#8715=CARTESIAN_POINT('Origin',(9.,1.,0.8));
#8716=CARTESIAN_POINT('',(8.85,1.,0.9));
#8717=CARTESIAN_POINT('Origin',(9.,1.,0.9));
#8718=CARTESIAN_POINT('',(8.85,1.,0.7));
#8719=CARTESIAN_POINT('',(8.85,1.,0.8));
#8720=CARTESIAN_POINT('Origin',(9.,1.,0.7));
#8721=CARTESIAN_POINT('Origin',(2.,0.,0.75));
#8722=CARTESIAN_POINT('',(1.7,3.67394039744206E-17,0.9));
#8723=CARTESIAN_POINT('Origin',(2.,0.,0.9));
#8724=CARTESIAN_POINT('',(1.7,3.67394039744206E-17,0.6));
#8725=CARTESIAN_POINT('',(1.7,3.67394039744206E-17,0.75));
#8726=CARTESIAN_POINT('Origin',(2.,0.,0.6));
#8727=CARTESIAN_POINT('Origin',(2.,0.,0.6));
#8728=CARTESIAN_POINT('',(1.83,-2.0818995585505E-17,0.6));
#8729=CARTESIAN_POINT('Origin',(2.,0.,0.6));
#8730=CARTESIAN_POINT('Origin',(10.,0.,0.75));
#8731=CARTESIAN_POINT('',(9.7,3.67394039744206E-17,0.9));
#8732=CARTESIAN_POINT('Origin',(10.,0.,0.9));
#8733=CARTESIAN_POINT('',(9.7,3.67394039744206E-17,0.6));
#8734=CARTESIAN_POINT('',(9.7,3.67394039744206E-17,0.75));
#8735=CARTESIAN_POINT('Origin',(10.,0.,0.6));
#8736=CARTESIAN_POINT('Origin',(10.,0.,0.6));
#8737=CARTESIAN_POINT('',(9.83,-2.0818995585505E-17,0.6));
#8738=CARTESIAN_POINT('Origin',(10.,0.,0.6));
#8739=CARTESIAN_POINT('Origin',(2.,0.,0.45));
#8740=CARTESIAN_POINT('',(1.83,-2.0818995585505E-17,0.32));
#8741=CARTESIAN_POINT('',(1.83,2.0818995585505E-17,0.45));
#8742=CARTESIAN_POINT('Origin',(2.,0.,0.32));
#8743=CARTESIAN_POINT('Origin',(10.,0.,0.45));
#8744=CARTESIAN_POINT('',(9.83,-2.0818995585505E-17,0.32));
#8745=CARTESIAN_POINT('',(9.83,2.0818995585505E-17,0.45));
#8746=CARTESIAN_POINT('Origin',(10.,0.,0.32));
#8747=CARTESIAN_POINT('Origin',(11.2,-0.62,0.32));
#8748=CARTESIAN_POINT('',(0.200274469199584,-0.62,0.));
#8749=CARTESIAN_POINT('',(0.217044958570157,-0.62,0.32));
#8750=CARTESIAN_POINT('',(0.223426876981161,-0.62,0.441774257530303));
#8751=CARTESIAN_POINT('',(0.,-0.62,0.));
#8752=CARTESIAN_POINT('',(8.63987299740311,-0.62,0.));
#8753=CARTESIAN_POINT('',(0.0167704893705732,-0.62,0.32));
#8754=CARTESIAN_POINT('',(0.0237009700302462,-0.62,0.452241448778892));
#8755=CARTESIAN_POINT('',(-0.1,-0.62,0.32));
#8756=CARTESIAN_POINT('Origin',(11.2,-0.62,0.32));
#8757=CARTESIAN_POINT('',(0.9,-0.62,0.32));
#8758=CARTESIAN_POINT('',(0.9,-0.62,0.));
#8759=CARTESIAN_POINT('',(0.9,-0.62,0.16));
#8760=CARTESIAN_POINT('',(1.1,-0.62,0.32));
#8761=CARTESIAN_POINT('',(-0.1,-0.62,0.32));
#8762=CARTESIAN_POINT('',(1.1,-0.62,0.));
#8763=CARTESIAN_POINT('',(1.1,-0.62,0.16));
#8764=CARTESIAN_POINT('',(8.63987299740311,-0.62,0.));
#8765=CARTESIAN_POINT('Origin',(11.2,-0.62,0.32));
#8766=CARTESIAN_POINT('',(3.9,-0.62,0.32));
#8767=CARTESIAN_POINT('',(3.9,-0.62,0.));
#8768=CARTESIAN_POINT('',(3.9,-0.62,0.16));
#8769=CARTESIAN_POINT('',(4.1,-0.62,0.32));
#8770=CARTESIAN_POINT('',(-0.1,-0.62,0.32));
#8771=CARTESIAN_POINT('',(4.1,-0.62,0.));
#8772=CARTESIAN_POINT('',(4.1,-0.62,0.16));
#8773=CARTESIAN_POINT('',(8.63987299740311,-0.62,0.));
#8774=CARTESIAN_POINT('Origin',(11.2,-0.62,0.32));
#8775=CARTESIAN_POINT('',(7.9,-0.62,0.32));
#8776=CARTESIAN_POINT('',(7.9,-0.62,0.));
#8777=CARTESIAN_POINT('',(7.9,-0.62,0.16));
#8778=CARTESIAN_POINT('',(8.1,-0.62,0.32));
#8779=CARTESIAN_POINT('',(-0.1,-0.62,0.32));
#8780=CARTESIAN_POINT('',(8.1,-0.62,0.));
#8781=CARTESIAN_POINT('',(8.1,-0.62,0.16));
#8782=CARTESIAN_POINT('',(8.63987299740311,-0.62,0.));
#8783=CARTESIAN_POINT('Origin',(-0.0999999999999996,0.62,0.32));
#8784=CARTESIAN_POINT('',(0.217044958570158,0.62,0.32));
#8785=CARTESIAN_POINT('',(0.200274469199586,0.62,0.));
#8786=CARTESIAN_POINT('',(0.207951231396534,0.62,0.146481348799182));
#8787=CARTESIAN_POINT('',(0.0167704893705736,0.62,0.32));
#8788=CARTESIAN_POINT('',(11.2,0.62,0.32));
#8789=CARTESIAN_POINT('',(0.,0.62,0.));
#8790=CARTESIAN_POINT('',(0.00822532444561912,0.62,0.156948540047771));
#8791=CARTESIAN_POINT('',(2.98987299740311,0.62,0.));
#8792=CARTESIAN_POINT('Origin',(-0.0999999999999996,0.62,0.32));
#8793=CARTESIAN_POINT('',(0.9,0.62,0.));
#8794=CARTESIAN_POINT('',(0.9,0.62,0.32));
#8795=CARTESIAN_POINT('',(0.9,0.62,0.16));
#8796=CARTESIAN_POINT('',(1.1,0.62,0.));
#8797=CARTESIAN_POINT('',(2.98987299740311,0.62,0.));
#8798=CARTESIAN_POINT('',(1.1,0.62,0.32));
#8799=CARTESIAN_POINT('',(1.1,0.62,0.16));
#8800=CARTESIAN_POINT('',(11.2,0.62,0.32));
#8801=CARTESIAN_POINT('Origin',(-0.0999999999999996,0.62,0.32));
#8802=CARTESIAN_POINT('',(3.9,0.62,0.));
#8803=CARTESIAN_POINT('',(3.9,0.62,0.32));
#8804=CARTESIAN_POINT('',(3.9,0.62,0.16));
#8805=CARTESIAN_POINT('',(4.1,0.62,0.));
#8806=CARTESIAN_POINT('',(2.98987299740311,0.62,0.));
#8807=CARTESIAN_POINT('',(4.1,0.62,0.32));
#8808=CARTESIAN_POINT('',(4.1,0.62,0.16));
#8809=CARTESIAN_POINT('',(11.2,0.62,0.32));
#8810=CARTESIAN_POINT('Origin',(5.55,0.,0.32));
#8811=CARTESIAN_POINT('',(1.6,-4.89858719658941E-17,0.32));
#8812=CARTESIAN_POINT('Origin',(2.,0.,0.32));
#8813=CARTESIAN_POINT('Origin',(5.55,0.,0.32));
#8814=CARTESIAN_POINT('',(9.6,-4.89858719658942E-17,0.32));
#8815=CARTESIAN_POINT('Origin',(10.,0.,0.32));
#8816=CARTESIAN_POINT('Origin',(5.55,0.,0.32));
#8817=CARTESIAN_POINT('',(0.217044958570157,-0.7,0.32));
#8818=CARTESIAN_POINT('',(0.0167704893705731,-0.7,0.32));
#8819=CARTESIAN_POINT('Origin',(5.55,0.,0.32));
#8820=CARTESIAN_POINT('',(0.9,0.724814814814815,0.32));
#8821=CARTESIAN_POINT('',(1.1,-0.724814814814815,0.32));
#8822=CARTESIAN_POINT('Origin',(5.55,0.,0.32));
#8823=CARTESIAN_POINT('',(3.9,0.883148148148148,0.32));
#8824=CARTESIAN_POINT('',(4.1,-0.883148148148148,0.32));
#8825=CARTESIAN_POINT('Origin',(5.55,0.,0.32));
#8826=CARTESIAN_POINT('',(7.9,0.62,0.32));
#8827=CARTESIAN_POINT('',(7.9,0.886851851851852,0.32));
#8828=CARTESIAN_POINT('',(8.1,0.62,0.32));
#8829=CARTESIAN_POINT('',(11.2,0.62,0.32));
#8830=CARTESIAN_POINT('',(8.1,-0.886851851851852,0.32));
#8831=CARTESIAN_POINT('Origin',(-0.0999999999999996,0.62,0.32));
#8832=CARTESIAN_POINT('',(7.9,0.62,0.));
#8833=CARTESIAN_POINT('',(7.9,0.62,0.16));
#8834=CARTESIAN_POINT('',(8.1,0.62,0.));
#8835=CARTESIAN_POINT('',(2.98987299740311,0.62,0.));
#8836=CARTESIAN_POINT('',(8.1,0.62,0.16));
#8837=CARTESIAN_POINT('Origin',(11.2,1.53779953703704,0.));
#8838=CARTESIAN_POINT('',(11.2,1.47592264243751,0.));
#8839=CARTESIAN_POINT('',(11.2,-1.47592264243751,0.));
#8840=CARTESIAN_POINT('',(11.2,1.53779953703704,0.));
#8841=CARTESIAN_POINT('',(11.2,-1.44160695250311,0.605635447211793));
#8842=CARTESIAN_POINT('Ctrl Pts',(11.2,-1.44160695250311,0.605635447211793));
#8843=CARTESIAN_POINT('Ctrl Pts',(11.2,-1.44733381480461,0.504614841520655));
#8844=CARTESIAN_POINT('Ctrl Pts',(11.2,-1.45305922122436,0.403593539811385));
#8845=CARTESIAN_POINT('Ctrl Pts',(11.2,-1.46449774781658,0.201715464978033));
#8846=CARTESIAN_POINT('Ctrl Pts',(11.2,-1.47021094199039,0.100857470386242));
#8847=CARTESIAN_POINT('Ctrl Pts',(11.2,-1.47592264243751,0.));
#8848=CARTESIAN_POINT('',(11.2,-1.3413305091784,0.7));
#8849=CARTESIAN_POINT('Ctrl Pts',(11.2,-1.34133050917871,0.7));
#8850=CARTESIAN_POINT('Ctrl Pts',(11.2,-1.34927184579059,0.7));
#8851=CARTESIAN_POINT('Ctrl Pts',(11.1999981201149,-1.35715077597425,0.699006225306896));
#8852=CARTESIAN_POINT('Ctrl Pts',(11.1999964866412,-1.36482619101963,0.697118463987577));
#8853=CARTESIAN_POINT('Ctrl Pts',(11.1999955714568,-1.36912648693643,0.696060810134936));
#8854=CARTESIAN_POINT('Ctrl Pts',(11.1999947385598,-1.37336294684024,0.694721504600825));
#8855=CARTESIAN_POINT('Ctrl Pts',(11.1999942054834,-1.37750904339755,0.693111246644731));
#8856=CARTESIAN_POINT('Ctrl Pts',(11.1999932489192,-1.38494889279378,0.690221763364053));
#8857=CARTESIAN_POINT('Ctrl Pts',(11.1999934335488,-1.39201911070639,0.686493604183975));
#8858=CARTESIAN_POINT('Ctrl Pts',(11.1999946360439,-1.39857284316731,0.682006025455124));
#8859=CARTESIAN_POINT('Ctrl Pts',(11.1999952980149,-1.40218065925828,0.679535622697003));
#8860=CARTESIAN_POINT('Ctrl Pts',(11.1999962427007,-1.40563167682227,0.676834205328214));
#8861=CARTESIAN_POINT('Ctrl Pts',(11.1999970766466,-1.40889738828709,0.673909521834337));
#8862=CARTESIAN_POINT('Ctrl Pts',(11.1999978839828,-1.41205889660265,0.671078159882768));
#8863=CARTESIAN_POINT('Ctrl Pts',(11.1999985961359,-1.41502771690814,0.668054510912379));
#8864=CARTESIAN_POINT('Ctrl Pts',(11.1999985943254,-1.41778154893794,0.664849526385156));
#8865=CARTESIAN_POINT('Ctrl Pts',(11.1999985909468,-1.42292039881534,0.658868793295219));
#8866=CARTESIAN_POINT('Ctrl Pts',(11.1999963776609,-1.42731355725865,0.652257958652517));
#8867=CARTESIAN_POINT('Ctrl Pts',(11.1999956369,-1.43089859237711,0.645180832176479));
#8868=CARTESIAN_POINT('Ctrl Pts',(11.1999955610412,-1.43126572346771,0.644456088045497));
#8869=CARTESIAN_POINT('Ctrl Pts',(11.1999954968237,-1.43162433912915,0.643726434786758));
#8870=CARTESIAN_POINT('Ctrl Pts',(11.1999954455063,-1.43197434355081,0.642992037678167));
#8871=CARTESIAN_POINT('Ctrl Pts',(11.1999949451572,-1.43538691836834,0.635831599341589));
#8872=CARTESIAN_POINT('Ctrl Pts',(11.1999960935741,-1.43794480573841,0.628305806294037));
#8873=CARTESIAN_POINT('Ctrl Pts',(11.1999977538348,-1.43959303921538,0.620581877990282));
#8874=CARTESIAN_POINT('Ctrl Pts',(11.1999988103007,-1.44064185190664,0.615666946856702));
#8875=CARTESIAN_POINT('Ctrl Pts',(11.1999999935832,-1.44132148083109,0.610671141596651));
#8876=CARTESIAN_POINT('Ctrl Pts',(11.1999999950647,-1.44160695392865,0.605635447210179));
#8877=CARTESIAN_POINT('',(11.2,1.34133050917871,0.7));
#8878=CARTESIAN_POINT('',(11.2,0.768899768518519,0.7));
#8879=CARTESIAN_POINT('',(11.2,1.44160695250311,0.605635447211793));
#8880=CARTESIAN_POINT('Ctrl Pts',(11.1999999950647,1.44160695392865,0.605635447210179));
#8881=CARTESIAN_POINT('Ctrl Pts',(11.1999999927383,1.44115867123275,0.613543073794128));
#8882=CARTESIAN_POINT('Ctrl Pts',(11.199997327584,1.43974095598264,0.62135504174347));
#8883=CARTESIAN_POINT('Ctrl Pts',(11.1999961426836,1.43743894790867,0.628911795513178));
#8884=CARTESIAN_POINT('Ctrl Pts',(11.1999954950047,1.43618064644969,0.633042395401645));
#8885=CARTESIAN_POINT('Ctrl Pts',(11.1999951984378,1.4346571631488,0.63709676955888));
#8886=CARTESIAN_POINT('Ctrl Pts',(11.1999953420225,1.43287614971348,0.641047046155727));
#8887=CARTESIAN_POINT('Ctrl Pts',(11.1999956050472,1.42961361303411,0.648283331988978));
#8888=CARTESIAN_POINT('Ctrl Pts',(11.1999975633633,1.42552584716917,0.655091209244077));
#8889=CARTESIAN_POINT('Ctrl Pts',(11.1999983488166,1.42067941835906,0.661308913390503));
#8890=CARTESIAN_POINT('Ctrl Pts',(11.1999985007599,1.41974189284539,0.662511707551344));
#8891=CARTESIAN_POINT('Ctrl Pts',(11.1999985958742,1.41877583892185,0.663692344451305));
#8892=CARTESIAN_POINT('Ctrl Pts',(11.1999985956185,1.41778154881703,0.664849526385225));
#8893=CARTESIAN_POINT('Ctrl Pts',(11.199998595152,1.41596832836708,0.666959801783445));
#8894=CARTESIAN_POINT('Ctrl Pts',(11.1999982799021,1.41406123008998,0.668992111776222));
#8895=CARTESIAN_POINT('Ctrl Pts',(11.1999978412043,1.41206657472189,0.670943322037058));
#8896=CARTESIAN_POINT('Ctrl Pts',(11.1999965906985,1.40638082038708,0.676505236328724));
#8897=CARTESIAN_POINT('Ctrl Pts',(11.1999945592311,1.40005057587654,0.681348449922958));
#8898=CARTESIAN_POINT('Ctrl Pts',(11.1999938793032,1.39324090595796,0.685420973467861));
#8899=CARTESIAN_POINT('Ctrl Pts',(11.1999934424014,1.38886521116801,0.68803785802621));
#8900=CARTESIAN_POINT('Ctrl Pts',(11.1999934711477,1.38429057260668,0.690335857752236));
#8901=CARTESIAN_POINT('Ctrl Pts',(11.1999939665515,1.37955471147715,0.692291686537622));
#8902=CARTESIAN_POINT('Ctrl Pts',(11.1999947349645,1.37220899016913,0.695325342464331));
#8903=CARTESIAN_POINT('Ctrl Pts',(11.1999966395725,1.36455954597093,0.697503651902993));
#8904=CARTESIAN_POINT('Ctrl Pts',(11.1999981885915,1.35675452105021,0.698758058199902));
#8905=CARTESIAN_POINT('Ctrl Pts',(11.1999991983045,1.35166689148409,0.699575730741489));
#8906=CARTESIAN_POINT('Ctrl Pts',(11.2,1.34651254223162,0.7));
#8907=CARTESIAN_POINT('Ctrl Pts',(11.2,1.34133050917871,0.7));
#8908=CARTESIAN_POINT('Ctrl Pts',(11.2,1.47592264243751,0.));
#8909=CARTESIAN_POINT('Ctrl Pts',(11.2,1.47021025951677,0.100869521536925));
#8910=CARTESIAN_POINT('Ctrl Pts',(11.2,1.4644963825062,0.20173956751342));
#8911=CARTESIAN_POINT('Ctrl Pts',(11.2,1.45305785520703,0.403617642353031));
#8912=CARTESIAN_POINT('Ctrl Pts',(11.2,1.44733313162379,0.50462689268162));
#8913=CARTESIAN_POINT('Ctrl Pts',(11.2,1.44160695250311,0.605635447211793));
#8914=CARTESIAN_POINT('Origin',(8.1,-1.7737037037037,0.));
#8915=CARTESIAN_POINT('',(8.1,1.69866351109718,0.));
#8916=CARTESIAN_POINT('',(8.1,-1.7737037037037,0.));
#8917=CARTESIAN_POINT('',(8.1,1.66641703131627,0.605314487869832));
#8918=CARTESIAN_POINT('Ctrl Pts',(8.1,1.66641703131627,0.605314487869832));
#8919=CARTESIAN_POINT('Ctrl Pts',(8.1,1.67178339996556,0.504592280948055));
#8920=CARTESIAN_POINT('Ctrl Pts',(8.1,1.67714947719849,0.403869246528492));
#8921=CARTESIAN_POINT('Ctrl Pts',(8.1,1.68789827452893,0.202098297941347));
#8922=CARTESIAN_POINT('Ctrl Pts',(8.1,1.69328107955938,0.101048748975501));
#8923=CARTESIAN_POINT('Ctrl Pts',(8.1,1.69866351109718,0.));
#8924=CARTESIAN_POINT('',(8.1,1.56644778183753,0.7));
#8925=CARTESIAN_POINT('Ctrl Pts',(8.0999999986552,1.56644778212326,0.7));
#8926=CARTESIAN_POINT('Ctrl Pts',(8.10000000155239,1.57436337254628,0.699999999341293));
#8927=CARTESIAN_POINT('Ctrl Pts',(8.09999905041684,1.58221543358893,0.699005989267703));
#8928=CARTESIAN_POINT('Ctrl Pts',(8.09999821745812,1.58986365929578,0.697118696434997));
#8929=CARTESIAN_POINT('Ctrl Pts',(8.099997748439,1.59417019217574,0.69605600700222));
#8930=CARTESIAN_POINT('Ctrl Pts',(8.09999731997616,1.59841215407948,0.694709061504878));
#8931=CARTESIAN_POINT('Ctrl Pts',(8.09999704681388,1.60256279759721,0.693088866918468));
#8932=CARTESIAN_POINT('Ctrl Pts',(8.09999655811104,1.60998853482381,0.690190246691698));
#8933=CARTESIAN_POINT('Ctrl Pts',(8.09999665589197,1.61704187682962,0.686451534538094));
#8934=CARTESIAN_POINT('Ctrl Pts',(8.09999726576867,1.62357667434142,0.681954089017224));
#8935=CARTESIAN_POINT('Ctrl Pts',(8.09999760196939,1.62717904774802,0.679474826559159));
#8936=CARTESIAN_POINT('Ctrl Pts',(8.09999808150314,1.6306235748906,0.676764109620253));
#8937=CARTESIAN_POINT('Ctrl Pts',(8.09999850764167,1.63388182210815,0.673830012183301));
#8938=CARTESIAN_POINT('Ctrl Pts',(8.09999892160867,1.637047006066,0.670979719520364));
#8939=CARTESIAN_POINT('Ctrl Pts',(8.09999928906958,1.640017230617,0.667935813742119));
#8940=CARTESIAN_POINT('Ctrl Pts',(8.09999928944056,1.64277007752663,0.664709670235875));
#8941=CARTESIAN_POINT('Ctrl Pts',(8.09999929012967,1.64788359851353,0.658716982277737));
#8942=CARTESIAN_POINT('Ctrl Pts',(8.09999816327153,1.65225000627493,0.652096887528603));
#8943=CARTESIAN_POINT('Ctrl Pts',(8.09999778355904,1.65580927004486,0.645014643130784));
#8944=CARTESIAN_POINT('Ctrl Pts',(8.09999774450894,1.65617530914943,0.644286296325024));
#8945=CARTESIAN_POINT('Ctrl Pts',(8.09999771143612,1.65653277094855,0.643553041785202));
#8946=CARTESIAN_POINT('Ctrl Pts',(8.0999976850083,1.65688156115921,0.642815048027137));
#8947=CARTESIAN_POINT('Ctrl Pts',(8.09999742811004,1.66027206465027,0.635641192980042));
#8948=CARTESIAN_POINT('Ctrl Pts',(8.09999800724182,1.66280786743682,0.628104262855387));
#8949=CARTESIAN_POINT('Ctrl Pts',(8.09999885110511,1.66443535430957,0.620372450280339));
#8950=CARTESIAN_POINT('Ctrl Pts',(8.09999939164969,1.6654778563549,0.615419764910946));
#8951=CARTESIAN_POINT('Ctrl Pts',(8.1,1.66614680274328,0.610386449940169));
#8952=CARTESIAN_POINT('Ctrl Pts',(8.1,1.66641703131627,0.605314487869832));
#8953=CARTESIAN_POINT('',(8.1,-1.56644778183827,0.7));
#8954=CARTESIAN_POINT('',(8.1,-0.886851851851852,0.7));
#8955=CARTESIAN_POINT('',(8.1,-1.66641703131627,0.605314487869832));
#8956=CARTESIAN_POINT('Ctrl Pts',(8.1,-1.66641703131627,0.605314487869832));
#8957=CARTESIAN_POINT('Ctrl Pts',(8.1,-1.66599546653325,0.613226902778437));
#8958=CARTESIAN_POINT('Ctrl Pts',(8.09999864563672,-1.66460605882141,0.621047760783158));
#8959=CARTESIAN_POINT('Ctrl Pts',(8.09999804140045,-1.66233302739118,0.628616817026045));
#8960=CARTESIAN_POINT('Ctrl Pts',(8.09999770486592,-1.66106704316887,0.632832467392296));
#8961=CARTESIAN_POINT('Ctrl Pts',(8.0999975536836,-1.65952595995304,0.636970042829054));
#8962=CARTESIAN_POINT('Ctrl Pts',(8.09999763427866,-1.65771765414013,0.640999885518982));
#8963=CARTESIAN_POINT('Ctrl Pts',(8.09999777898787,-1.65447082344915,0.64823550729937));
#8964=CARTESIAN_POINT('Ctrl Pts',(8.09999878245444,-1.65040085231772,0.655045563401426));
#8965=CARTESIAN_POINT('Ctrl Pts',(8.09999917121848,-1.64557198994432,0.661267087195486));
#8966=CARTESIAN_POINT('Ctrl Pts',(8.09999924425118,-1.6446648462537,0.662435854416292));
#8967=CARTESIAN_POINT('Ctrl Pts',(8.09999928944999,-1.64373079085321,0.663583781603691));
#8968=CARTESIAN_POINT('Ctrl Pts',(8.09999928890117,-1.64277007755202,0.664709670235858));
#8969=CARTESIAN_POINT('Ctrl Pts',(8.09999928782175,-1.64088054556816,0.666924069243459));
#8970=CARTESIAN_POINT('Ctrl Pts',(8.09999911129818,-1.63888792496677,0.66905326411728));
#8971=CARTESIAN_POINT('Ctrl Pts',(8.09999887085824,-1.63679941630975,0.671093569621172));
#8972=CARTESIAN_POINT('Ctrl Pts',(8.09999821641022,-1.6311147520694,0.676647030794692));
#8973=CARTESIAN_POINT('Ctrl Pts',(8.0999972000003,-1.62478663867955,0.681482189379454));
#8974=CARTESIAN_POINT('Ctrl Pts',(8.09999686812141,-1.6179789612855,0.685544965666037));
#8975=CARTESIAN_POINT('Ctrl Pts',(8.09999665686968,-1.61364565292072,0.68813105508359));
#8976=CARTESIAN_POINT('Ctrl Pts',(8.09999667786582,-1.6091170759025,0.690403516124292));
#8977=CARTESIAN_POINT('Ctrl Pts',(8.0999969341683,-1.60442977212996,0.692339085768374));
#8978=CARTESIAN_POINT('Ctrl Pts',(8.09999733452329,-1.59710801128849,0.695362524980696));
#8979=CARTESIAN_POINT('Ctrl Pts',(8.09999831212369,-1.58948382509795,0.697531565976904));
#8980=CARTESIAN_POINT('Ctrl Pts',(8.09999909563861,-1.58170429192971,0.698776637084609));
#8981=CARTESIAN_POINT('Ctrl Pts',(8.09999960249138,-1.57667174192468,0.69958206878261));
#8982=CARTESIAN_POINT('Ctrl Pts',(8.1000000005313,-1.5715735875011,0.699999999573449));
#8983=CARTESIAN_POINT('Ctrl Pts',(8.0999999986552,-1.56644778212326,0.7));
#8984=CARTESIAN_POINT('',(8.1,-1.69866351109718,0.));
#8985=CARTESIAN_POINT('Ctrl Pts',(8.1,-1.69866351109718,0.));
#8986=CARTESIAN_POINT('Ctrl Pts',(8.1,-1.69328105674055,0.101049177371948));
#8987=CARTESIAN_POINT('Ctrl Pts',(8.1,-1.68789822886868,0.202099155105557));
#8988=CARTESIAN_POINT('Ctrl Pts',(8.1,-1.67714943151225,0.403870104074094));
#8989=CARTESIAN_POINT('Ctrl Pts',(8.1,-1.67178337712185,0.50459270970527));
#8990=CARTESIAN_POINT('Ctrl Pts',(8.1,-1.66641703131627,0.605314487869832));
#8991=CARTESIAN_POINT('',(8.1,-1.7737037037037,0.));
#8992=CARTESIAN_POINT('Origin',(4.1,-1.7662962962963,0.));
#8993=CARTESIAN_POINT('',(4.1,1.70113889814581,0.));
#8994=CARTESIAN_POINT('',(4.1,-1.7662962962963,0.));
#8995=CARTESIAN_POINT('',(4.1,1.66887738702937,0.605315322680072));
#8996=CARTESIAN_POINT('Ctrl Pts',(4.1,1.66887738702937,0.605315322680072));
#8997=CARTESIAN_POINT('Ctrl Pts',(4.1,1.67424235111642,0.50466767694528));
#8998=CARTESIAN_POINT('Ctrl Pts',(4.1,1.67960699363804,0.404019058341251));
#8999=CARTESIAN_POINT('Ctrl Pts',(4.1,1.69036079691899,0.202247931921761));
#9000=CARTESIAN_POINT('Ctrl Pts',(4.1,1.6957500571643,0.101123491803998));
#9001=CARTESIAN_POINT('Ctrl Pts',(4.1,1.70113889814581,0.));
#9002=CARTESIAN_POINT('',(4.1,1.56887583540973,0.7));
#9003=CARTESIAN_POINT('Ctrl Pts',(4.1,1.56887583540973,0.7));
#9004=CARTESIAN_POINT('Ctrl Pts',(4.1,1.57679416129392,0.7));
#9005=CARTESIAN_POINT('Ctrl Pts',(4.10000107724674,1.58464912207822,0.699006028000541));
#9006=CARTESIAN_POINT('Ctrl Pts',(4.10000201939527,1.59230028572239,0.697118705459362));
#9007=CARTESIAN_POINT('Ctrl Pts',(4.10000255022779,1.59661116283941,0.696055335763773));
#9008=CARTESIAN_POINT('Ctrl Pts',(4.10000303435977,1.60085740028891,0.694707333985525));
#9009=CARTESIAN_POINT('Ctrl Pts',(4.10000334030352,1.60501217339351,0.693085708041268));
#9010=CARTESIAN_POINT('Ctrl Pts',(4.10000388718746,1.61243895913315,0.690187001388783));
#9011=CARTESIAN_POINT('Ctrl Pts',(4.10000376557609,1.61949349263125,0.686448444730844));
#9012=CARTESIAN_POINT('Ctrl Pts',(4.10000306534783,1.6260295229635,0.681951159450519));
#9013=CARTESIAN_POINT('Ctrl Pts',(4.10000267892397,1.62963645835533,0.679469313954069));
#9014=CARTESIAN_POINT('Ctrl Pts',(4.10000213012555,1.63308521926452,0.676755517937216));
#9015=CARTESIAN_POINT('Ctrl Pts',(4.1000016436875,1.63634725251217,0.673817835781739));
#9016=CARTESIAN_POINT('Ctrl Pts',(4.10000117237165,1.63950787692018,0.67097147916344));
#9017=CARTESIAN_POINT('Ctrl Pts',(4.10000075597222,1.64247408874941,0.667932078875657));
#9018=CARTESIAN_POINT('Ctrl Pts',(4.10000075698646,1.64522354659423,0.664710927554201));
#9019=CARTESIAN_POINT('Ctrl Pts',(4.1000007588733,1.65033845220459,0.658718515269377));
#9020=CARTESIAN_POINT('Ctrl Pts',(4.10000204656096,1.65470614797426,0.652098486008568));
#9021=CARTESIAN_POINT('Ctrl Pts',(4.10000248678323,1.65826650381873,0.645016049251367));
#9022=CARTESIAN_POINT('Ctrl Pts',(4.10000253228732,1.65863452415637,0.644283964909082));
#9023=CARTESIAN_POINT('Ctrl Pts',(4.10000257095464,1.65899387729575,0.643546919913709));
#9024=CARTESIAN_POINT('Ctrl Pts',(4.10000260201855,1.65934446736461,0.642805085364403));
#9025=CARTESIAN_POINT('Ctrl Pts',(4.10000290242009,1.66273482600052,0.635631222228741));
#9026=CARTESIAN_POINT('Ctrl Pts',(4.10000225562543,1.66527033938482,0.628094305374488));
#9027=CARTESIAN_POINT('Ctrl Pts',(4.10000130084992,1.66689736875237,0.62036252267401));
#9028=CARTESIAN_POINT('Ctrl Pts',(4.10000068968835,1.66793884687677,0.615413329558163));
#9029=CARTESIAN_POINT('Ctrl Pts',(4.09999999901039,1.66860722297681,0.610383627857512));
#9030=CARTESIAN_POINT('Ctrl Pts',(4.09999999630223,1.66887738567036,0.60531532268817));
#9031=CARTESIAN_POINT('',(4.1,-1.56887583540947,0.7));
#9032=CARTESIAN_POINT('',(4.1,-0.883148148148148,0.7));
#9033=CARTESIAN_POINT('',(4.1,-1.66887738702937,0.605315322680072));
#9034=CARTESIAN_POINT('Ctrl Pts',(4.09999999630223,-1.66887738567036,0.60531532268817));
#9035=CARTESIAN_POINT('Ctrl Pts',(4.10000000053001,-1.66845562780346,0.613227583070809));
#9036=CARTESIAN_POINT('Ctrl Pts',(4.10000153668442,-1.66706589531621,0.621048261667561));
#9037=CARTESIAN_POINT('Ctrl Pts',(4.10000221487211,-1.66479240287642,0.628617079688242));
#9038=CARTESIAN_POINT('Ctrl Pts',(4.10000259231836,-1.6635270876889,0.632829515245766));
#9039=CARTESIAN_POINT('Ctrl Pts',(4.10000275805793,-1.66198703315979,0.636963972243471));
#9040=CARTESIAN_POINT('Ctrl Pts',(4.10000266178038,-1.66018010017296,0.640990858692597));
#9041=CARTESIAN_POINT('Ctrl Pts',(4.10000248876893,-1.65693302887506,0.648227201990446));
#9042=CARTESIAN_POINT('Ctrl Pts',(4.10000134097948,-1.65286254930452,0.655037795911226));
#9043=CARTESIAN_POINT('Ctrl Pts',(4.100000893742,-1.6480330317196,0.661259713776781));
#9044=CARTESIAN_POINT('Ctrl Pts',(4.10000080951506,-1.647123502594,0.662431469633614));
#9045=CARTESIAN_POINT('Ctrl Pts',(4.10000075717637,-1.6461869221106,0.663582276554164));
#9046=CARTESIAN_POINT('Ctrl Pts',(4.10000075728519,-1.64522354661022,0.66471092755419));
#9047=CARTESIAN_POINT('Ctrl Pts',(4.10000075749815,-1.64333815989002,0.666919768869269));
#9048=CARTESIAN_POINT('Ctrl Pts',(4.1000009568795,-1.64135017761634,0.669043797975229));
#9049=CARTESIAN_POINT('Ctrl Pts',(4.10000122972053,-1.63926675509047,0.671079366787198));
#9050=CARTESIAN_POINT('Ctrl Pts',(4.10000197419082,-1.6335819569127,0.676633591976433));
#9051=CARTESIAN_POINT('Ctrl Pts',(4.10000313643093,-1.62725355063421,0.681469444454218));
#9052=CARTESIAN_POINT('Ctrl Pts',(4.1000035230587,-1.62044557755217,0.685533082105531));
#9053=CARTESIAN_POINT('Ctrl Pts',(4.10000376939409,-1.61610795658125,0.688122181633714));
#9054=CARTESIAN_POINT('Ctrl Pts',(4.10000375220654,-1.61157469281532,0.690397125746379));
#9055=CARTESIAN_POINT('Ctrl Pts',(4.10000346632868,-1.60688245467732,0.692334655286926));
#9056=CARTESIAN_POINT('Ctrl Pts',(4.10000302008581,-1.59955807566073,0.695359054367588));
#9057=CARTESIAN_POINT('Ctrl Pts',(4.1000019139068,-1.59193114173487,0.69752894708864));
#9058=CARTESIAN_POINT('Ctrl Pts',(4.10000102635309,-1.58414888227482,0.698774888159427));
#9059=CARTESIAN_POINT('Ctrl Pts',(4.10000045177616,-1.57911086966871,0.699581474839467));
#9060=CARTESIAN_POINT('Ctrl Pts',(4.1,-1.57400716417114,0.7));
#9061=CARTESIAN_POINT('Ctrl Pts',(4.1,-1.56887583540973,0.7));
#9062=CARTESIAN_POINT('',(4.1,-1.70113889814582,0.));
#9063=CARTESIAN_POINT('Ctrl Pts',(4.1,-1.70113889814582,0.));
#9064=CARTESIAN_POINT('Ctrl Pts',(4.1,-1.69575004793467,0.101123665001254));
#9065=CARTESIAN_POINT('Ctrl Pts',(4.1,-1.69036077845691,0.202248278345555));
#9066=CARTESIAN_POINT('Ctrl Pts',(4.1,-1.67960697517202,0.404019404791024));
#9067=CARTESIAN_POINT('Ctrl Pts',(4.1,-1.67424234188296,0.504667850166609));
#9068=CARTESIAN_POINT('Ctrl Pts',(4.1,-1.66887738702937,0.605315322680072));
#9069=CARTESIAN_POINT('',(4.1,-1.7662962962963,0.));
#9070=CARTESIAN_POINT('Origin',(1.1,-1.44962962962963,0.));
#9071=CARTESIAN_POINT('',(1.1,1.39262953588351,0.));
#9072=CARTESIAN_POINT('',(1.1,-1.44962962962963,0.));
#9073=CARTESIAN_POINT('',(1.10000000000005,1.35674377243284,0.605845626926786));
#9074=CARTESIAN_POINT('Ctrl Pts',(1.10000000000005,1.35674377243284,0.605845626926786));
#9075=CARTESIAN_POINT('Ctrl Pts',(1.10000000000005,1.36273568520883,0.504787121979256));
#9076=CARTESIAN_POINT('Ctrl Pts',(1.1,1.36872466312622,0.403727404115485));
#9077=CARTESIAN_POINT('Ctrl Pts',(1.1,1.38068651056748,0.201779555185378));
#9078=CARTESIAN_POINT('Ctrl Pts',(1.1,1.38665951284069,0.10088935150083));
#9079=CARTESIAN_POINT('Ctrl Pts',(1.1,1.39262953588351,0.));
#9080=CARTESIAN_POINT('',(1.1,1.25565664448622,0.7));
#9081=CARTESIAN_POINT('Ctrl Pts',(1.1,1.25565664448621,0.7));
#9082=CARTESIAN_POINT('Ctrl Pts',(1.1,1.26365753466764,0.700000000000001));
#9083=CARTESIAN_POINT('Ctrl Pts',(1.10000312127109,1.27160078819195,0.699008097631352));
#9084=CARTESIAN_POINT('Ctrl Pts',(1.10000579554281,1.27934333527045,0.697120485426804));
#9085=CARTESIAN_POINT('Ctrl Pts',(1.10000709386889,1.28310224676699,0.696204072889075));
#9086=CARTESIAN_POINT('Ctrl Pts',(1.10000828779753,1.28681383019745,0.695075712339665));
#9087=CARTESIAN_POINT('Ctrl Pts',(1.10000913303706,1.29046059826345,0.693742188764313));
#9088=CARTESIAN_POINT('Ctrl Pts',(1.10001087659788,1.29798315455626,0.69099139518989));
#9089=CARTESIAN_POINT('Ctrl Pts',(1.10001086910546,1.30515375246939,0.687398976275641));
#9090=CARTESIAN_POINT('Ctrl Pts',(1.10000899624477,1.31182501206943,0.683041610144935));
#9091=CARTESIAN_POINT('Ctrl Pts',(1.10000779407289,1.31610723164143,0.680244657298552));
#9092=CARTESIAN_POINT('Ctrl Pts',(1.10000585478529,1.32018349952736,0.677131483611404));
#9093=CARTESIAN_POINT('Ctrl Pts',(1.10000422180804,1.32400796947387,0.673713330684339));
#9094=CARTESIAN_POINT('Ctrl Pts',(1.10000291018178,1.3270798280974,0.670967830603965));
#9095=CARTESIAN_POINT('Ctrl Pts',(1.10000180047651,1.32997084712789,0.668041731908725));
#9096=CARTESIAN_POINT('Ctrl Pts',(1.10000182449184,1.33266034096938,0.664944387470286));
#9097=CARTESIAN_POINT('Ctrl Pts',(1.10000187074845,1.33784065079383,0.65897850512594));
#9098=CARTESIAN_POINT('Ctrl Pts',(1.10000564109429,1.34227630326151,0.652378581761819));
#9099=CARTESIAN_POINT('Ctrl Pts',(1.10000696187003,1.34590032739451,0.645305437365917));
#9100=CARTESIAN_POINT('Ctrl Pts',(1.100007110355,1.34630774940504,0.644510256482779));
#9101=CARTESIAN_POINT('Ctrl Pts',(1.10000723579819,1.34670486410349,0.643709073603569));
#9102=CARTESIAN_POINT('Ctrl Pts',(1.10000733566964,1.34709153749004,0.642902104572485));
#9103=CARTESIAN_POINT('Ctrl Pts',(1.10000822022419,1.35051627708745,0.63575483535061));
#9104=CARTESIAN_POINT('Ctrl Pts',(1.10000635568239,1.35308446649167,0.628241602461225));
#9105=CARTESIAN_POINT('Ctrl Pts',(1.10000361780323,1.35473867947858,0.620527690691125));
#9106=CARTESIAN_POINT('Ctrl Pts',(1.1000019043033,1.35577396762308,0.615699943921843));
#9107=CARTESIAN_POINT('Ctrl Pts',(1.09999998677418,1.35645041192828,0.610792997969602));
#9108=CARTESIAN_POINT('Ctrl Pts',(1.09999997754868,1.35674374570294,0.605845627052288));
#9109=CARTESIAN_POINT('',(1.1,-1.25565664448622,0.7));
#9110=CARTESIAN_POINT('',(1.1,-0.724814814814815,0.7));
#9111=CARTESIAN_POINT('',(1.10000000000005,-1.35674377243284,0.605845626926786));
#9112=CARTESIAN_POINT('Ctrl Pts',(1.09999997754868,-1.35674374570294,0.605845627052288));
#9113=CARTESIAN_POINT('Ctrl Pts',(1.09999999227748,-1.35627542940044,0.613744255356351));
#9114=CARTESIAN_POINT('Ctrl Pts',(1.1000044245081,-1.35483313756702,0.621542702113576));
#9115=CARTESIAN_POINT('Ctrl Pts',(1.10000632213307,-1.3525036790266,0.629082464357584));
#9116=CARTESIAN_POINT('Ctrl Pts',(1.1000073336739,-1.3512619466217,0.633101581650771));
#9117=CARTESIAN_POINT('Ctrl Pts',(1.10000777634458,-1.34976719347553,0.637047225321331));
#9118=CARTESIAN_POINT('Ctrl Pts',(1.10000752568741,-1.34802684471036,0.640893844816285));
#9119=CARTESIAN_POINT('Ctrl Pts',(1.10000705344834,-1.3447480208661,0.648140890909733));
#9120=CARTESIAN_POINT('Ctrl Pts',(1.10000374385205,-1.34063788586045,0.654954534019122));
#9121=CARTESIAN_POINT('Ctrl Pts',(1.10000230512149,-1.33576793982513,0.661175616324976));
#9122=CARTESIAN_POINT('Ctrl Pts',(1.10000200863552,-1.33476436716076,0.662457623989879));
#9123=CARTESIAN_POINT('Ctrl Pts',(1.10000181701501,-1.33372836971272,0.663714393476354));
#9124=CARTESIAN_POINT('Ctrl Pts',(1.10000180919237,-1.33266033853372,0.664944387472089));
#9125=CARTESIAN_POINT('Ctrl Pts',(1.10000179685332,-1.33097567746633,0.666884520904953));
#9126=CARTESIAN_POINT('Ctrl Pts',(1.10000223926429,-1.32921133126375,0.668758058859172));
#9127=CARTESIAN_POINT('Ctrl Pts',(1.10000288715521,-1.32737234926393,0.670562692084704));
#9128=CARTESIAN_POINT('Ctrl Pts',(1.10000489069569,-1.32168547392559,0.676143347135183));
#9129=CARTESIAN_POINT('Ctrl Pts',(1.10000845923633,-1.31535192007569,0.681005160308095));
#9130=CARTESIAN_POINT('Ctrl Pts',(1.1000097672184,-1.30853956043085,0.685101187995272));
#9131=CARTESIAN_POINT('Ctrl Pts',(1.10001062829021,-1.30405484229164,0.687797688271992));
#9132=CARTESIAN_POINT('Ctrl Pts',(1.10001067755751,-1.29936155475819,0.690161668140197));
#9133=CARTESIAN_POINT('Ctrl Pts',(1.10000992106221,-1.29450057597768,0.692169783635984));
#9134=CARTESIAN_POINT('Ctrl Pts',(1.10000876843985,-1.28709422081189,0.695229417764685));
#9135=CARTESIAN_POINT('Ctrl Pts',(1.100005676647,-1.27938091857402,0.69743146309387));
#9136=CARTESIAN_POINT('Ctrl Pts',(1.10000309801581,-1.2715114871423,0.698709794160748));
#9137=CARTESIAN_POINT('Ctrl Pts',(1.10000138449209,-1.26628217885177,0.699559256705032));
#9138=CARTESIAN_POINT('Ctrl Pts',(1.1,-1.26098326598685,0.700000000000001));
#9139=CARTESIAN_POINT('Ctrl Pts',(1.1,-1.25565664448621,0.7));
#9140=CARTESIAN_POINT('',(1.1,-1.39262953588351,0.));
#9141=CARTESIAN_POINT('Ctrl Pts',(1.1,-1.39262953588351,0.));
#9142=CARTESIAN_POINT('Ctrl Pts',(1.1,-1.38665944902278,0.100890429980357));
#9143=CARTESIAN_POINT('Ctrl Pts',(1.1,-1.38068638286488,0.201781712214768));
#9144=CARTESIAN_POINT('Ctrl Pts',(1.1,-1.36872453529477,0.403729561179669));
#9145=CARTESIAN_POINT('Ctrl Pts',(1.10000000000005,-1.3627356212621,0.504788200493074));
#9146=CARTESIAN_POINT('Ctrl Pts',(1.10000000000005,-1.35674377243284,0.605845626926786));
#9147=CARTESIAN_POINT('',(1.1,-1.44962962962963,0.));
#9148=CARTESIAN_POINT('Origin',(0.199725906950915,-1.4,-0.0104671912485888));
#9149=CARTESIAN_POINT('',(0.200274469199584,1.15262458915154,1.38777878078145E-17));
#9150=CARTESIAN_POINT('',(0.200274469199585,-0.7,0.));
#9151=CARTESIAN_POINT('',(0.231993417893744,1.12115139781563,0.605233595624295));
#9152=CARTESIAN_POINT('Ctrl Pts',(0.200274469199584,1.15262458915154,-5.50774703622636E-17));
#9153=CARTESIAN_POINT('Ctrl Pts',(0.210847451072758,1.1421331482829,0.201744512318911));
#9154=CARTESIAN_POINT('Ctrl Pts',(0.221420433966108,1.13164208276446,0.403489044103923));
#9155=CARTESIAN_POINT('Ctrl Pts',(0.231993417893744,1.12115139781563,0.605233595624295));
#9156=CARTESIAN_POINT('',(0.231993417893744,-1.12115139781563,0.605233595624295));
#9157=CARTESIAN_POINT('',(0.231993417893744,-0.7,0.605233595624295));
#9158=CARTESIAN_POINT('',(0.200274469199584,-1.15262458915154,1.38777878078145E-17));
#9159=CARTESIAN_POINT('Ctrl Pts',(0.231993417893744,-1.12115139781563,0.605233595624295));
#9160=CARTESIAN_POINT('Ctrl Pts',(0.221420433966108,-1.13164208276446,0.403489044103923));
#9161=CARTESIAN_POINT('Ctrl Pts',(0.210847451072758,-1.1421331482829,0.201744512318911));
#9162=CARTESIAN_POINT('Ctrl Pts',(0.200274469199584,-1.15262458915154,-6.67868538251071E-17));
#9163=CARTESIAN_POINT('',(0.200274469199585,-0.7,0.));
#9164=CARTESIAN_POINT('Origin',(6.07974599480623,0.,0.));
#9165=CARTESIAN_POINT('Ctrl Pts',(8.1,-1.69866351109718,4.37041895728907E-16));
#9166=CARTESIAN_POINT('Ctrl Pts',(8.9524267631348,-1.65897367198627,1.20944032620455E-7));
#9167=CARTESIAN_POINT('Ctrl Pts',(9.80407798130771,-1.59837060538327,2.76830114922109E-8));
#9168=CARTESIAN_POINT('Ctrl Pts',(10.6537697771985,-1.52488560579501,1.03413542584124E-8));
#9169=CARTESIAN_POINT('Ctrl Pts',(10.8359404901627,-1.50913069933138,6.62336842220622E-9));
#9170=CARTESIAN_POINT('Ctrl Pts',(11.0180211259896,-1.49278349820154,3.93228299510406E-9));
#9171=CARTESIAN_POINT('Ctrl Pts',(11.2000000002909,-1.47592264092474,-3.0227174540096E-11));
#9172=CARTESIAN_POINT('Ctrl Pts',(11.2000000002909,1.47592264092474,-3.02272213335841E-11));
#9173=CARTESIAN_POINT('Ctrl Pts',(10.4240589919717,1.54781576943643,1.68591524001238E-8));
#9174=CARTESIAN_POINT('Ctrl Pts',(9.64626799696257,1.61037563220813,6.17878738288937E-8));
#9175=CARTESIAN_POINT('Ctrl Pts',(8.86753211358286,1.65747704847969,5.27022751808308E-8));
#9176=CARTESIAN_POINT('Ctrl Pts',(8.61177933690776,1.67294611604661,4.97183789310355E-8));
#9177=CARTESIAN_POINT('Ctrl Pts',(8.35592462822135,1.68674740550612,3.63007687033005E-8));
#9178=CARTESIAN_POINT('Ctrl Pts',(8.1,1.69866351109718,3.71000138306103E-16));
#9179=CARTESIAN_POINT('',(7.9,1.70758761671949,0.));
#9180=CARTESIAN_POINT('',(7.9,1.7737037037037,0.));
#9181=CARTESIAN_POINT('Ctrl Pts',(7.90000000036908,1.70758761645525,-3.06814577203155E-11));
#9182=CARTESIAN_POINT('Ctrl Pts',(7.26247716501442,1.73478515342832,3.65175246633048E-8));
#9183=CARTESIAN_POINT('Ctrl Pts',(6.624575449312,1.74993328406844,-3.04558542439636E-7));
#9184=CARTESIAN_POINT('Ctrl Pts',(5.98677261990733,1.74972113442148,-3.1918790057331E-7));
#9185=CARTESIAN_POINT('Ctrl Pts',(5.35540610719671,1.74951112565922,-3.33669628155763E-7));
#9186=CARTESIAN_POINT('Ctrl Pts',(4.72663057529054,1.73425216511322,1.21151810208783E-7));
#9187=CARTESIAN_POINT('Ctrl Pts',(4.10000000045307,1.7011388979176,-4.27317258673188E-11));
#9188=CARTESIAN_POINT('',(3.9,1.68995649764597,0.));
#9189=CARTESIAN_POINT('',(3.9,1.7662962962963,0.));
#9190=CARTESIAN_POINT('Ctrl Pts',(3.9,1.68995649764597,-1.6113354923472E-17));
#9191=CARTESIAN_POINT('Ctrl Pts',(2.96252047830716,1.63464572816558,-1.61179993858831E-17));
#9192=CARTESIAN_POINT('Ctrl Pts',(2.02971500398675,1.53866944530133,-1.61823222708931E-17));
#9193=CARTESIAN_POINT('Ctrl Pts',(1.1,1.39262953588351,-1.60717230190728E-17));
#9194=CARTESIAN_POINT('',(0.9,1.3604297237941,0.));
#9195=CARTESIAN_POINT('',(0.9,1.44962962962963,0.));
#9196=CARTESIAN_POINT('',(0.28146619846596,1.25073018526678,0.));
#9197=CARTESIAN_POINT('Ctrl Pts',(0.899999999999963,1.36042972379409,2.53412200078296E-14));
#9198=CARTESIAN_POINT('Ctrl Pts',(0.693681964344164,1.32640030945436,-1.68820282978727E-7));
#9199=CARTESIAN_POINT('Ctrl Pts',(0.487510176034459,1.28986876146525,1.95094241611213E-11));
#9200=CARTESIAN_POINT('Ctrl Pts',(0.281466198465954,1.25073018526678,9.09211941846344E-16));
#9201=CARTESIAN_POINT('Ctrl Pts',(0.28146619846596,1.25073018526678,4.90059381963448E-17));
#9202=CARTESIAN_POINT('Ctrl Pts',(0.273672142824666,1.24924968434803,-1.60851827685828E-11));
#9203=CARTESIAN_POINT('Ctrl Pts',(0.266112037439191,1.2468180315926,-2.29735811958388E-6));
#9204=CARTESIAN_POINT('Ctrl Pts',(0.258922416881026,1.24354471831116,-3.39045428380668E-6));
#9205=CARTESIAN_POINT('Ctrl Pts',(0.254316658841251,1.24144779416325,-4.09070493067818E-6));
#9206=CARTESIAN_POINT('Ctrl Pts',(0.249862973385875,1.23900427835211,-4.3601744978078E-6));
#9207=CARTESIAN_POINT('Ctrl Pts',(0.245601965247185,1.23623285256398,-4.0505643599354E-6));
#9208=CARTESIAN_POINT('Ctrl Pts',(0.238945660500109,1.23190348870705,-3.5669089987193E-6));
#9209=CARTESIAN_POINT('Ctrl Pts',(0.232836306411817,1.22682685988243,-1.47564048465526E-6));
#9210=CARTESIAN_POINT('Ctrl Pts',(0.227416445112993,1.2210931256102,-3.43092614100725E-7));
#9211=CARTESIAN_POINT('Ctrl Pts',(0.225957664245637,1.21954986437275,-3.82620891408318E-8));
#9212=CARTESIAN_POINT('Ctrl Pts',(0.224549002474426,1.21795876469157,1.76022586487844E-7));
#9213=CARTESIAN_POINT('Ctrl Pts',(0.223193686986583,1.21632111005909,2.01577349231486E-7));
#9214=CARTESIAN_POINT('Ctrl Pts',(0.221344954485829,1.21408724984631,2.36435595047204E-7));
#9215=CARTESIAN_POINT('Ctrl Pts',(0.219595448227346,1.21176677459781,-7.7718209010198E-8));
#9216=CARTESIAN_POINT('Ctrl Pts',(0.217948412504407,1.20936721934621,-5.08402878561E-7));
#9217=CARTESIAN_POINT('Ctrl Pts',(0.213467776427723,1.20283941082417,-1.68004793834142E-6));
#9218=CARTESIAN_POINT('Ctrl Pts',(0.20978887558685,1.19579640990262,-3.43350901357988E-6));
#9219=CARTESIAN_POINT('Ctrl Pts',(0.206958221875648,1.18840352636746,-3.67425174897535E-6));
#9220=CARTESIAN_POINT('Ctrl Pts',(0.206193447398199,1.18640614723908,-3.7392946395744E-6));
#9221=CARTESIAN_POINT('Ctrl Pts',(0.205490847532167,1.18438308363371,-3.7149036306613E-6));
#9222=CARTESIAN_POINT('Ctrl Pts',(0.204851940804359,1.18233735619935,-3.6037364623937E-6));
#9223=CARTESIAN_POINT('Ctrl Pts',(0.202492508448082,1.17478264548698,-3.19320484275276E-6));
#9224=CARTESIAN_POINT('Ctrl Pts',(0.201019195184615,1.16698811697394,-1.36638523817118E-6));
#9225=CARTESIAN_POINT('Ctrl Pts',(0.200491965466086,1.15911075533121,-4.28455138775697E-7));
#9226=CARTESIAN_POINT('Ctrl Pts',(0.200347608840846,1.15695391685535,-1.71647870329038E-7));
#9227=CARTESIAN_POINT('Ctrl Pts',(0.200274469313241,1.15479080601565,-7.49035961899928E-12));
#9228=CARTESIAN_POINT('Ctrl Pts',(0.200274469199584,1.15262458915154,9.10729824887824E-18));
#9229=CARTESIAN_POINT('',(2.01407162049393E-18,1.15316892111334,2.77409355997279E-17));
#9230=CARTESIAN_POINT('',(0.,-1.4,0.));
#9231=CARTESIAN_POINT('',(0.243580684154574,1.44748675362873,2.77555756156289E-17));
#9232=CARTESIAN_POINT('Ctrl Pts',(0.243580684154575,1.44748675362873,-1.56125112837913E-16));
#9233=CARTESIAN_POINT('Ctrl Pts',(0.226022619058538,1.44415189332774,-6.74769223000006E-12));
#9234=CARTESIAN_POINT('Ctrl Pts',(0.208837776424359,1.43922483814223,-1.83343972289099E-6));
#9235=CARTESIAN_POINT('Ctrl Pts',(0.192216855517481,1.43283671850359,-2.37047811876899E-6));
#9236=CARTESIAN_POINT('Ctrl Pts',(0.175448307189507,1.42639185943196,-2.91228650265529E-6));
#9237=CARTESIAN_POINT('Ctrl Pts',(0.15925228528901,1.41845922211561,-2.09168970691363E-6));
#9238=CARTESIAN_POINT('Ctrl Pts',(0.143842215871583,1.4091253227419,-1.20497646612983E-7));
#9239=CARTESIAN_POINT('Ctrl Pts',(0.141154971457358,1.40749765525544,2.23243494969264E-7));
#9240=CARTESIAN_POINT('Ctrl Pts',(0.138491701959641,1.40582727297256,5.92673833856784E-7));
#9241=CARTESIAN_POINT('Ctrl Pts',(0.135853645420207,1.40411450883245,9.74556207071009E-7));
#9242=CARTESIAN_POINT('Ctrl Pts',(0.120686164410185,1.39426698768136,3.17018528370531E-6));
#9243=CARTESIAN_POINT('Ctrl Pts',(0.106484701177391,1.38310949089167,6.09567884445769E-6));
#9244=CARTESIAN_POINT('Ctrl Pts',(0.0934509959242968,1.37075049507673,5.10227143121889E-6));
#9245=CARTESIAN_POINT('Ctrl Pts',(0.0918301157095608,1.36921352217444,4.97873062758527E-6));
#9246=CARTESIAN_POINT('Ctrl Pts',(0.0902273306836925,1.36765791150105,4.78983320752683E-6));
#9247=CARTESIAN_POINT('Ctrl Pts',(0.0886430622088043,1.36608382581751,4.52250464763623E-6));
#9248=CARTESIAN_POINT('Ctrl Pts',(0.0755027622673366,1.35302798437193,2.30521792157715E-6));
#9249=CARTESIAN_POINT('Ctrl Pts',(0.0636322991078783,1.33870385142449,-4.95851449924696E-6));
#9250=CARTESIAN_POINT('Ctrl Pts',(0.0531272107863483,1.3233265665666,-1.07771754856876E-5));
#9251=CARTESIAN_POINT('Ctrl Pts',(0.0429100363670196,1.3083707283404,-1.64363639061758E-5));
#9252=CARTESIAN_POINT('Ctrl Pts',(0.0340657397255946,1.29253754778979,-2.07072841115287E-5));
#9253=CARTESIAN_POINT('Ctrl Pts',(0.026663056477648,1.27603964904139,-2.15377272154938E-5));
#9254=CARTESIAN_POINT('Ctrl Pts',(0.0217318501145713,1.26504977678014,-2.20909166714363E-5));
#9255=CARTESIAN_POINT('Ctrl Pts',(0.0174411483101006,1.25376411673155,-2.12025196266096E-5));
#9256=CARTESIAN_POINT('Ctrl Pts',(0.01382286588119,1.24224013948332,-1.91534441809703E-5));
#9257=CARTESIAN_POINT('Ctrl Pts',(0.00842668188255806,1.22505366970124,
-1.60975223868617E-5));
#9258=CARTESIAN_POINT('Ctrl Pts',(0.00456091079961661,1.20745571355567,
-1.03588883906395E-5));
#9259=CARTESIAN_POINT('Ctrl Pts',(0.0023097402764219,1.18964331095195,-5.71664032024866E-6));
#9260=CARTESIAN_POINT('Ctrl Pts',(0.00078319128522165,1.17756448131848,
-2.56866950429304E-6));
#9261=CARTESIAN_POINT('Ctrl Pts',(2.50028438421117E-9,1.16538650529032,
-1.91718613723104E-10));
#9262=CARTESIAN_POINT('Ctrl Pts',(-1.21430643318376E-17,1.15316892111333,
5.20417042793042E-18));
#9263=CARTESIAN_POINT('',(11.7295909468525,1.62672708026858,5.55111512312578E-17));
#9264=CARTESIAN_POINT('Ctrl Pts',(0.243580684154574,1.44748675362873,0.));
#9265=CARTESIAN_POINT('Ctrl Pts',(4.07225077172054,2.17467835246083,0.));
#9266=CARTESIAN_POINT('Ctrl Pts',(7.90092085928651,2.00057770191527,0.));
#9267=CARTESIAN_POINT('Ctrl Pts',(11.7295909468525,1.62672708026858,0.));
#9268=CARTESIAN_POINT('',(12.,1.32855945177638,-4.17473993839455E-17));
#9269=CARTESIAN_POINT('Ctrl Pts',(12.,1.32855945177638,2.42861286636753E-16));
#9270=CARTESIAN_POINT('Ctrl Pts',(11.9999999991614,1.34640852075174,-1.28298622986823E-11));
#9271=CARTESIAN_POINT('Ctrl Pts',(11.9983618543561,1.36418409382152,-2.22383001277967E-6));
#9272=CARTESIAN_POINT('Ctrl Pts',(11.9951861391139,1.38167870884165,-3.43465861540838E-6));
#9273=CARTESIAN_POINT('Ctrl Pts',(11.9919727904737,1.39938064150867,-4.65983598400874E-6));
#9274=CARTESIAN_POINT('Ctrl Pts',(11.9871848331028,1.41679645887758,-4.78742071954366E-6));
#9275=CARTESIAN_POINT('Ctrl Pts',(11.9808755917115,1.43370272794343,-3.5739118077222E-6));
#9276=CARTESIAN_POINT('Ctrl Pts',(11.9797611226834,1.43668906371449,-3.35955670324834E-6));
#9277=CARTESIAN_POINT('Ctrl Pts',(11.9785990681726,1.43965944485564,-3.11247275469786E-6));
#9278=CARTESIAN_POINT('Ctrl Pts',(11.9773895732386,1.44261255525912,-2.84353511336506E-6));
#9279=CARTESIAN_POINT('Ctrl Pts',(11.9705369081732,1.45934406518776,-1.31980853313606E-6));
#9280=CARTESIAN_POINT('Ctrl Pts',(11.9622259501015,1.47537448669426,1.24030492427686E-6));
#9281=CARTESIAN_POINT('Ctrl Pts',(11.9525330320198,1.49048867890869,8.79804099270529E-7));
#9282=CARTESIAN_POINT('Ctrl Pts',(11.9492586078121,1.49559449703792,7.58021100761347E-7));
#9283=CARTESIAN_POINT('Ctrl Pts',(11.9458260650319,1.50059560584699,2.73671093112169E-7));
#9284=CARTESIAN_POINT('Ctrl Pts',(11.9422371454499,1.50548309160802,-8.21070286398525E-7));
#9285=CARTESIAN_POINT('Ctrl Pts',(11.9335276940755,1.51734385321214,-3.47774636801117E-6));
#9286=CARTESIAN_POINT('Ctrl Pts',(11.923898315087,1.52853671512454,-9.61160164537397E-6));
#9287=CARTESIAN_POINT('Ctrl Pts',(11.9134480753511,1.53899918600446,-1.54908303532852E-5));
#9288=CARTESIAN_POINT('Ctrl Pts',(11.9006414429521,1.55182080751067,-2.26957483986032E-5));
#9289=CARTESIAN_POINT('Ctrl Pts',(11.8867118754531,1.56343792791748,-2.93307907620841E-5));
#9290=CARTESIAN_POINT('Ctrl Pts',(11.8718669715436,1.57375979462261,-3.2097080434168E-5));
#9291=CARTESIAN_POINT('Ctrl Pts',(11.8583226919989,1.58317731924447,-3.46210038525051E-5));
#9292=CARTESIAN_POINT('Ctrl Pts',(11.84401509256,1.59151672629289,-3.39892197405707E-5));
#9293=CARTESIAN_POINT('Ctrl Pts',(11.8290799708805,1.59867837245092,-3.04453078860132E-5));
#9294=CARTESIAN_POINT('Ctrl Pts',(11.8128282236205,1.60647136308226,-2.65889777530425E-5));
#9295=CARTESIAN_POINT('Ctrl Pts',(11.7959622791259,1.61280865470064,-1.93051308245346E-5));
#9296=CARTESIAN_POINT('Ctrl Pts',(11.7786680578171,1.61758555622507,-1.24065785496921E-5));
#9297=CARTESIAN_POINT('Ctrl Pts',(11.7626326571209,1.62201475420184,-6.0101616208217E-6));
#9298=CARTESIAN_POINT('Ctrl Pts',(11.7462278952123,1.62510256303752,-1.15598952599692E-10));
#9299=CARTESIAN_POINT('Ctrl Pts',(11.7295909468525,1.62672708026857,-1.01481323344643E-16));
#9300=CARTESIAN_POINT('',(12.,-1.32855945177638,-2.7831599589297E-17));
#9301=CARTESIAN_POINT('',(12.,1.6,0.));
#9302=CARTESIAN_POINT('',(11.7295909468525,-1.62672708026858,-2.77555756156289E-17));
#9303=CARTESIAN_POINT('Ctrl Pts',(11.7295909468525,-1.62672708026858,2.76688394418301E-16));
#9304=CARTESIAN_POINT('Ctrl Pts',(11.7473502233519,-1.62499297457843,3.63491969896433E-13));
#9305=CARTESIAN_POINT('Ctrl Pts',(11.7648769397846,-1.62163540491215,-2.46542030701863E-6));
#9306=CARTESIAN_POINT('Ctrl Pts',(11.7819744899096,-1.61677476461769,-3.87870576098494E-6));
#9307=CARTESIAN_POINT('Ctrl Pts',(11.799277951102,-1.61185558613358,-5.30901184740094E-6));
#9308=CARTESIAN_POINT('Ctrl Pts',(11.8161433440738,-1.60539638769883,-5.61072687595782E-6));
#9309=CARTESIAN_POINT('Ctrl Pts',(11.8323535184498,-1.59747214364331,-4.43708131311936E-6));
#9310=CARTESIAN_POINT('Ctrl Pts',(11.8351986841263,-1.59608130189932,-4.23108623901291E-6));
#9311=CARTESIAN_POINT('Ctrl Pts',(11.8380235988884,-1.59464521634493,-3.98890160078043E-6));
#9312=CARTESIAN_POINT('Ctrl Pts',(11.8408269920241,-1.59316415515964,-3.72087260345577E-6));
#9313=CARTESIAN_POINT('Ctrl Pts',(11.8568148563263,-1.58471760338924,-2.19229240409177E-6));
#9314=CARTESIAN_POINT('Ctrl Pts',(11.8719627312575,-1.57488689795395,5.08047814114288E-7));
#9315=CARTESIAN_POINT('Ctrl Pts',(11.8860639991294,-1.56376935451958,3.7910357452838E-7));
#9316=CARTESIAN_POINT('Ctrl Pts',(11.8908390360804,-1.5600046802233,3.35439876042474E-7));
#9317=CARTESIAN_POINT('Ctrl Pts',(11.8954938739134,-1.55609205312677,-6.31409548673105E-8));
#9318=CARTESIAN_POINT('Ctrl Pts',(11.9000197537765,-1.55203410647271,-1.07033715310124E-6));
#9319=CARTESIAN_POINT('Ctrl Pts',(11.9109521284419,-1.54223203603875,-3.50324446252274E-6));
#9320=CARTESIAN_POINT('Ctrl Pts',(11.9211333865357,-1.53158293117673,-9.37257606292525E-6));
#9321=CARTESIAN_POINT('Ctrl Pts',(11.9305114837192,-1.52019095639426,-1.50133174764804E-5));
#9322=CARTESIAN_POINT('Ctrl Pts',(11.9420285825687,-1.50620064502377,-2.19406264148308E-5));
#9323=CARTESIAN_POINT('Ctrl Pts',(11.9522379825693,-1.49120969914507,-2.8349487615449E-5));
#9324=CARTESIAN_POINT('Ctrl Pts',(11.9610699533786,-1.47543375940277,-3.10096306454085E-5));
#9325=CARTESIAN_POINT('Ctrl Pts',(11.9691383866925,-1.46102167397773,-3.34398002084833E-5));
#9326=CARTESIAN_POINT('Ctrl Pts',(11.976057247492,-1.44595309822982,-3.28127654573608E-5));
#9327=CARTESIAN_POINT('Ctrl Pts',(11.9817405815488,-1.43037347552767,-2.93737351251587E-5));
#9328=CARTESIAN_POINT('Ctrl Pts',(11.9879190063177,-1.41343666945002,-2.56351214921306E-5));
#9329=CARTESIAN_POINT('Ctrl Pts',(11.9925890154887,-1.39602986621001,-1.86015881889918E-5));
#9330=CARTESIAN_POINT('Ctrl Pts',(11.9956646601292,-1.37834843064327,-1.1951505214167E-5));
#9331=CARTESIAN_POINT('Ctrl Pts',(11.9985188379205,-1.36194017591583,-5.78027239782095E-6));
#9332=CARTESIAN_POINT('Ctrl Pts',(11.9999999979315,-1.34529424449622,-1.63143103698095E-10));
#9333=CARTESIAN_POINT('Ctrl Pts',(12.,-1.32855945177638,6.07153216591882E-17));
#9334=CARTESIAN_POINT('',(0.243580684154574,-1.44748675362873,-2.77555756156289E-17));
#9335=CARTESIAN_POINT('Ctrl Pts',(11.7295909468525,-1.62672708026858,0.));
#9336=CARTESIAN_POINT('Ctrl Pts',(7.90092085928651,-2.00057770191527,0.));
#9337=CARTESIAN_POINT('Ctrl Pts',(4.07225077172054,-2.17467835246083,0.));
#9338=CARTESIAN_POINT('Ctrl Pts',(0.243580684154574,-1.44748675362873,0.));
#9339=CARTESIAN_POINT('',(-2.01407162049393E-18,-1.15316892111334,-2.77409355997279E-17));
#9340=CARTESIAN_POINT('Ctrl Pts',(-1.45716771982052E-16,-1.15316892111333,
-8.67361737988404E-17));
#9341=CARTESIAN_POINT('Ctrl Pts',(1.25998894435939E-9,-1.17105087373522,
-1.90287520688926E-11));
#9342=CARTESIAN_POINT('Ctrl Pts',(0.00163339464743996,-1.18886359576077,
-1.42965894531121E-6));
#9343=CARTESIAN_POINT('Ctrl Pts',(0.00480727841906161,-1.20639511031145,
-1.64093682142839E-6));
#9344=CARTESIAN_POINT('Ctrl Pts',(0.00800796397580062,-1.22407466931478,
-1.8539988284852E-6));
#9345=CARTESIAN_POINT('Ctrl Pts',(0.0127756311263789,-1.24146980201313,
-7.66483898132055E-7));
#9346=CARTESIAN_POINT('Ctrl Pts',(0.0190655400899108,-1.25835467436912,
1.24978183846727E-6));
#9347=CARTESIAN_POINT('Ctrl Pts',(0.0201762582672253,-1.26133632875492,
1.60582880463507E-6));
#9348=CARTESIAN_POINT('Ctrl Pts',(0.0213345630164365,-1.2643020159517,1.98173645466097E-6));
#9349=CARTESIAN_POINT('Ctrl Pts',(0.022540357064946,-1.26725040777374,2.36324320385681E-6));
#9350=CARTESIAN_POINT('Ctrl Pts',(0.0293845669280623,-1.28398578013164,
4.5287143794027E-6));
#9351=CARTESIAN_POINT('Ctrl Pts',(0.0376942987862453,-1.30001720705818,
7.20349268724091E-6));
#9352=CARTESIAN_POINT('Ctrl Pts',(0.0474014865253391,-1.31512615530125,
5.82569015349308E-6));
#9353=CARTESIAN_POINT('Ctrl Pts',(0.0485928463173857,-1.31698047129067,
5.65659292531477E-6));
#9354=CARTESIAN_POINT('Ctrl Pts',(0.049805315173965,-1.3188208685659,5.4220814195758E-6));
#9355=CARTESIAN_POINT('Ctrl Pts',(0.0510388164126442,-1.32064691964073,
5.10992468070797E-6));
#9356=CARTESIAN_POINT('Ctrl Pts',(0.0614399911345998,-1.33604461498541,
2.47774509321499E-6));
#9357=CARTESIAN_POINT('Ctrl Pts',(0.0733332132114129,-1.35042574344132,
-5.3152380038924E-6));
#9358=CARTESIAN_POINT('Ctrl Pts',(0.0865238753361435,-1.36365441213776,
-1.1550981620978E-5));
#9359=CARTESIAN_POINT('Ctrl Pts',(0.0993129767592984,-1.37648036310613,
-1.75968917362996E-5));
#9360=CARTESIAN_POINT('Ctrl Pts',(0.113220041589059,-1.38812080263946,-2.21381304374214E-5));
#9361=CARTESIAN_POINT('Ctrl Pts',(0.128049501721596,-1.3984678073416,-2.30260298918279E-5));
#9362=CARTESIAN_POINT('Ctrl Pts',(0.137898881094142,-1.40534004502052,-2.36157518704412E-5));
#9363=CARTESIAN_POINT('Ctrl Pts',(0.148156110210342,-1.41164106947418,-2.26770903305374E-5));
#9364=CARTESIAN_POINT('Ctrl Pts',(0.158771208267938,-1.41732893485082,-2.05010084084185E-5));
#9365=CARTESIAN_POINT('Ctrl Pts',(0.174640735071984,-1.42583226958806,-1.72477751171679E-5));
#9366=CARTESIAN_POINT('Ctrl Pts',(0.191199787345415,-1.4329086754137,-1.11085100333009E-5));
#9367=CARTESIAN_POINT('Ctrl Pts',(0.208270835533445,-1.43843835369108,-6.12965879291162E-6));
#9368=CARTESIAN_POINT('Ctrl Pts',(0.219822542278978,-1.44218019901621,-2.76054936125183E-6));
#9369=CARTESIAN_POINT('Ctrl Pts',(0.231609382520684,-1.4452130041726,-1.10646384277296E-10));
#9370=CARTESIAN_POINT('Ctrl Pts',(0.243580684154575,-1.44748675362873,-8.67361737988404E-18));
#9371=CARTESIAN_POINT('',(0.,-1.4,0.));
#9372=CARTESIAN_POINT('',(0.28146619846596,-1.25073018526678,-1.38777878078145E-17));
#9373=CARTESIAN_POINT('Ctrl Pts',(0.200274469199584,-1.15262458915154,-4.38017677684144E-17));
#9374=CARTESIAN_POINT('Ctrl Pts',(0.200274469606231,-1.16056122076396,-2.67994619525583E-11));
#9375=CARTESIAN_POINT('Ctrl Pts',(0.201251993787099,-1.16844573575355,-2.06906772440415E-6));
#9376=CARTESIAN_POINT('Ctrl Pts',(0.203125250303271,-1.17612349127761,-3.03593176598444E-6));
#9377=CARTESIAN_POINT('Ctrl Pts',(0.204328175564463,-1.18105381768481,-3.65681052429326E-6));
#9378=CARTESIAN_POINT('Ctrl Pts',(0.205901645655995,-1.18589907428975,-3.87486521964464E-6));
#9379=CARTESIAN_POINT('Ctrl Pts',(0.207834893326199,-1.19061551412018,-3.56660141708203E-6));
#9380=CARTESIAN_POINT('Ctrl Pts',(0.210845733886816,-1.19796089907112,-3.08651126907409E-6));
#9381=CARTESIAN_POINT('Ctrl Pts',(0.214691665920849,-1.20490884791767,-1.13290501265697E-6));
#9382=CARTESIAN_POINT('Ctrl Pts',(0.219311372289421,-1.21130241743461,-1.88024479619773E-7));
#9383=CARTESIAN_POINT('Ctrl Pts',(0.220549822002528,-1.21301640393121,6.52788543367939E-8));
#9384=CARTESIAN_POINT('Ctrl Pts',(0.22184414018537,-1.21469042595737,2.26073670777299E-7));
#9385=CARTESIAN_POINT('Ctrl Pts',(0.223193686901845,-1.21632111014354,1.99977909429435E-7));
#9386=CARTESIAN_POINT('Ctrl Pts',(0.225054776233359,-1.21856990146355,1.63990609064731E-7));
#9387=CARTESIAN_POINT('Ctrl Pts',(0.227020882846909,-1.2207363067163,-2.2494482424301E-7));
#9388=CARTESIAN_POINT('Ctrl Pts',(0.229085096241527,-1.22281561536867,-7.25033596408456E-7));
#9389=CARTESIAN_POINT('Ctrl Pts',(0.234663732853057,-1.22843504764494,-2.07654770860772E-6));
#9390=CARTESIAN_POINT('Ctrl Pts',(0.240898147116973,-1.23336261820331,-3.93931381885212E-6));
#9391=CARTESIAN_POINT('Ctrl Pts',(0.247634917667946,-1.2375211924479,-4.15647360184107E-6));
#9392=CARTESIAN_POINT('Ctrl Pts',(0.24944409362824,-1.23863798757926,-4.21479238469909E-6));
#9393=CARTESIAN_POINT('Ctrl Pts',(0.251289686356224,-1.23969909864123,-4.17584617698396E-6));
#9394=CARTESIAN_POINT('Ctrl Pts',(0.253169062337335,-1.24070249413235,-4.04352721072409E-6));
#9395=CARTESIAN_POINT('Ctrl Pts',(0.260147540238377,-1.24442829106235,-3.55220190316667E-6));
#9396=CARTESIAN_POINT('Ctrl Pts',(0.267526846148503,-1.24732811138375,-1.51439637010182E-6));
#9397=CARTESIAN_POINT('Ctrl Pts',(0.275164162321015,-1.24931347733136,-4.73394739174148E-7));
#9398=CARTESIAN_POINT('Ctrl Pts',(0.277246452424842,-1.24985478107889,-1.89568936341825E-7));
#9399=CARTESIAN_POINT('Ctrl Pts',(0.27934803608603,-1.25032783487679,-4.20368826828312E-12));
#9400=CARTESIAN_POINT('Ctrl Pts',(0.28146619846596,-1.25073018526678,1.2793585635329E-17));
#9401=CARTESIAN_POINT('',(0.9,-1.3604297237941,0.));
#9402=CARTESIAN_POINT('Ctrl Pts',(0.281466198465954,-1.25073018526678,9.63150999927498E-16));
#9403=CARTESIAN_POINT('Ctrl Pts',(0.487510152792939,-1.28986875705046,1.95065110193295E-11));
#9404=CARTESIAN_POINT('Ctrl Pts',(0.693681940810289,-1.32640030557063,-1.68784634270162E-7));
#9405=CARTESIAN_POINT('Ctrl Pts',(0.899999999999961,-1.36042972379409,2.52314774976951E-14));
#9406=CARTESIAN_POINT('',(0.9,1.44962962962963,0.));
#9407=CARTESIAN_POINT('',(3.9,-1.68995649764597,0.));
#9408=CARTESIAN_POINT('Ctrl Pts',(1.1,-1.39262953588351,-2.05019623674552E-17));
#9409=CARTESIAN_POINT('Ctrl Pts',(2.02971449277185,-1.53866936499954,-2.04062575199768E-17));
#9410=CARTESIAN_POINT('Ctrl Pts',(2.96251993741879,-1.63464569625347,-2.05230086706555E-17));
#9411=CARTESIAN_POINT('Ctrl Pts',(3.9,-1.68995649764597,-2.05203881127908E-17));
#9412=CARTESIAN_POINT('',(3.9,1.7662962962963,0.));
#9413=CARTESIAN_POINT('',(7.9,-1.70758761671949,0.));
#9414=CARTESIAN_POINT('Ctrl Pts',(4.10000000045307,-1.7011388979176,-4.27317380631109E-11));
#9415=CARTESIAN_POINT('Ctrl Pts',(4.72643887491804,-1.7342420350347,1.20853286712337E-7));
#9416=CARTESIAN_POINT('Ctrl Pts',(5.35502164560988,-1.74950180199062,-3.33551248611792E-7));
#9417=CARTESIAN_POINT('Ctrl Pts',(5.98619394951577,-1.74972093772735,-3.1920111515717E-7));
#9418=CARTESIAN_POINT('Ctrl Pts',(6.62418968669829,-1.74994244248134,-3.0469584628258E-7));
#9419=CARTESIAN_POINT('Ctrl Pts',(7.26228442347589,-1.73479337602516,3.6583895104054E-8));
#9420=CARTESIAN_POINT('Ctrl Pts',(7.90000000036908,-1.70758761645525,-3.06816097140251E-11));
#9421=CARTESIAN_POINT('',(7.9,1.7737037037037,0.));
#9422=CARTESIAN_POINT('',(11.4,-1.45718524058191,0.));
#9423=CARTESIAN_POINT('',(11.7095901160181,-1.42740242188993,1.38777878078145E-17));
#9424=CARTESIAN_POINT('Ctrl Pts',(11.4000000008084,-1.45718524050535,1.02728155843002E-16));
#9425=CARTESIAN_POINT('Ctrl Pts',(11.5032315878449,-1.44740895658952,-1.62414911853346E-10));
#9426=CARTESIAN_POINT('Ctrl Pts',(11.6064290066394,-1.43747657129068,3.17212713797596E-13));
#9427=CARTESIAN_POINT('Ctrl Pts',(11.7095901160181,-1.42740242188993,-1.31135713082882E-16));
#9428=CARTESIAN_POINT('',(11.7997255308004,-1.32801330383774,0.));
#9429=CARTESIAN_POINT('Ctrl Pts',(11.7095901160181,-1.42740242188993,-9.19403442267708E-17));
#9430=CARTESIAN_POINT('Ctrl Pts',(11.7174875668098,-1.42663119997609,-1.06723531187443E-12));
#9431=CARTESIAN_POINT('Ctrl Pts',(11.7252481284326,-1.42489860698852,-1.31351091787008E-6));
#9432=CARTESIAN_POINT('Ctrl Pts',(11.7327147629935,-1.4222933789697,-1.57347087725304E-6));
#9433=CARTESIAN_POINT('Ctrl Pts',(11.7375034508718,-1.42062252930751,-1.7401948673154E-6));
#9434=CARTESIAN_POINT('Ctrl Pts',(11.742171336984,-1.41859157258352,-1.52962160850981E-6));
#9435=CARTESIAN_POINT('Ctrl Pts',(11.7466731630754,-1.4162133745499,-1.06822103866601E-6));
#9436=CARTESIAN_POINT('Ctrl Pts',(11.7538080604269,-1.41244419322064,-3.36952074275293E-7));
#9437=CARTESIAN_POINT('Ctrl Pts',(11.7604421378066,-1.40785009750528,1.23525126371337E-6));
#9438=CARTESIAN_POINT('Ctrl Pts',(11.7664060685299,-1.40250292630552,-7.85770423176645E-8));
#9439=CARTESIAN_POINT('Ctrl Pts',(11.7700505374369,-1.39923534992309,-8.81437879006801E-7));
#9440=CARTESIAN_POINT('Ctrl Pts',(11.7734443324447,-1.39568546479044,-2.84121358692309E-6));
#9441=CARTESIAN_POINT('Ctrl Pts',(11.7765701913309,-1.39188797822873,-4.73246891796253E-6));
#9442=CARTESIAN_POINT('Ctrl Pts',(11.7816218974528,-1.38575085342217,-7.78893003218221E-6));
#9443=CARTESIAN_POINT('Ctrl Pts',(11.7859196635778,-1.3790373064984,-1.04294718165207E-5));
#9444=CARTESIAN_POINT('Ctrl Pts',(11.7894058487846,-1.37190723377291,-1.0649753115785E-5));
#9445=CARTESIAN_POINT('Ctrl Pts',(11.7909886780302,-1.36866997385604,-1.07497672177443E-5));
#9446=CARTESIAN_POINT('Ctrl Pts',(11.7924036476919,-1.36534638272796,-1.04045251440782E-5));
#9447=CARTESIAN_POINT('Ctrl Pts',(11.7936422141268,-1.36194984358789,-9.67400732978531E-6));
#9448=CARTESIAN_POINT('Ctrl Pts',(11.7963517531347,-1.35451943450186,-8.0758964348484E-6));
#9449=CARTESIAN_POINT('Ctrl Pts',(11.7981920551596,-1.34681816044402,-4.45435127417515E-6));
#9450=CARTESIAN_POINT('Ctrl Pts',(11.7990923524223,-1.33899256731255,-1.99131993767782E-6));
#9451=CARTESIAN_POINT('Ctrl Pts',(11.7995108157868,-1.33535518645399,-8.46488755312323E-7));
#9452=CARTESIAN_POINT('Ctrl Pts',(11.7997255306472,-1.33169069466208,-1.20180646731727E-11));
#9453=CARTESIAN_POINT('Ctrl Pts',(11.7997255308004,-1.32801330383774,1.56125112837913E-17));
#9454=CARTESIAN_POINT('',(11.7997255308004,1.32801330383774,-1.38777878078145E-17));
#9455=CARTESIAN_POINT('',(11.7997255308004,0.8,0.));
#9456=CARTESIAN_POINT('',(11.7095901160181,1.42740242188993,1.38777878078145E-17));
#9457=CARTESIAN_POINT('Ctrl Pts',(11.7997255308004,1.32801330383774,3.29597460435593E-17));
#9458=CARTESIAN_POINT('Ctrl Pts',(11.7997255306701,1.33594993357028,-3.19998942079111E-12));
#9459=CARTESIAN_POINT('Ctrl Pts',(11.7987557313351,1.34384388324515,-1.1738056914779E-6));
#9460=CARTESIAN_POINT('Ctrl Pts',(11.7968890528831,1.35153020534854,-1.35082478761126E-6));
#9461=CARTESIAN_POINT('Ctrl Pts',(11.7956902940742,1.35646627043222,-1.46450435604653E-6));
#9462=CARTESIAN_POINT('Ctrl Pts',(11.7941204989552,1.36131691981906,-1.21679535622301E-6));
#9463=CARTESIAN_POINT('Ctrl Pts',(11.7921880664813,1.36603565236267,-7.51718013047842E-7));
#9464=CARTESIAN_POINT('Ctrl Pts',(11.7891321441143,1.37349779167052,-1.62510435539431E-8));
#9465=CARTESIAN_POINT('Ctrl Pts',(11.7852081688769,1.38054242009704,1.47305143123643E-6));
#9466=CARTESIAN_POINT('Ctrl Pts',(11.7804707482717,1.38699431162271,4.31295153147674E-8));
#9467=CARTESIAN_POINT('Ctrl Pts',(11.7775673564694,1.39094843993989,-8.33217322910001E-7));
#9468=CARTESIAN_POINT('Ctrl Pts',(11.774357304366,1.39467961749964,-2.88177890715362E-6));
#9469=CARTESIAN_POINT('Ctrl Pts',(11.7708736118052,1.39816709864095,-4.85419454747415E-6));
#9470=CARTESIAN_POINT('Ctrl Pts',(11.7652557092992,1.40379111072049,-8.03496856102318E-6));
#9471=CARTESIAN_POINT('Ctrl Pts',(11.7589908599241,1.40872063947841,-1.07717451179728E-5));
#9472=CARTESIAN_POINT('Ctrl Pts',(11.7522324303862,1.41288246393566,-1.10093962897399E-5));
#9473=CARTESIAN_POINT('Ctrl Pts',(11.7491699691574,1.41476832010531,-1.11170836593312E-5));
#9474=CARTESIAN_POINT('Ctrl Pts',(11.7460056456443,1.41649603445901,-1.07652933077188E-5));
#9475=CARTESIAN_POINT('Ctrl Pts',(11.7427518690514,1.41805582819498,-1.00150721194158E-5));
#9476=CARTESIAN_POINT('Ctrl Pts',(11.7356218627913,1.421473806899,-8.37111113549047E-6));
#9477=CARTESIAN_POINT('Ctrl Pts',(11.7281378774234,1.42405291512428,-4.62166314666036E-6));
#9478=CARTESIAN_POINT('Ctrl Pts',(11.7204387731059,1.42570834923663,-2.06587013620581E-6));
#9479=CARTESIAN_POINT('Ctrl Pts',(11.7168648812537,1.42647679479109,-8.79481766934018E-7));
#9480=CARTESIAN_POINT('Ctrl Pts',(11.7132443218769,1.42704557200794,-8.45784208685192E-12));
#9481=CARTESIAN_POINT('Ctrl Pts',(11.7095901160181,1.42740242188993,2.53703308361608E-17));
#9482=CARTESIAN_POINT('',(11.4,1.45718524058191,0.));
#9483=CARTESIAN_POINT('Ctrl Pts',(11.7095901160181,1.42740242188993,-2.09644042577228E-16));
#9484=CARTESIAN_POINT('Ctrl Pts',(11.6064290073882,1.43747657121756,3.16925904777201E-13));
#9485=CARTESIAN_POINT('Ctrl Pts',(11.5032315885351,1.44740895652415,-1.62368751268212E-10));
#9486=CARTESIAN_POINT('Ctrl Pts',(11.4000000008083,1.45718524050537,-7.57963810214684E-17));
#9487=CARTESIAN_POINT('',(11.4,-1.53779953703704,0.));
#9488=CARTESIAN_POINT('Origin',(10.,0.,0.));
#9489=CARTESIAN_POINT('',(9.6,-4.89858719658942E-17,0.7));
#9490=CARTESIAN_POINT('Origin',(10.,0.,0.7));
#9491=CARTESIAN_POINT('',(9.6,-4.89858719658942E-17,0.));
#9492=CARTESIAN_POINT('Origin',(2.,0.,0.));
#9493=CARTESIAN_POINT('',(1.6,-4.89858719658941E-17,0.7));
#9494=CARTESIAN_POINT('Origin',(2.,0.,0.7));
#9495=CARTESIAN_POINT('',(1.6,-4.89858719658941E-17,0.));
#9496=CARTESIAN_POINT('Origin',(11.4,-1.53779953703704,0.));
#9497=CARTESIAN_POINT('',(11.4,-1.4227102204299,0.605660349289938));
#9498=CARTESIAN_POINT('Ctrl Pts',(11.4,-1.45718524058191,0.));
#9499=CARTESIAN_POINT('Ctrl Pts',(11.4,-1.45144762186897,0.100853500740053));
#9500=CARTESIAN_POINT('Ctrl Pts',(11.4,-1.44570843451869,0.201707502489292));
#9501=CARTESIAN_POINT('Ctrl Pts',(11.4,-1.43421679834229,0.403593890565801));
#9502=CARTESIAN_POINT('Ctrl Pts',(11.4,-1.42846427656079,0.504627461196798));
#9503=CARTESIAN_POINT('Ctrl Pts',(11.4,-1.4227102204299,0.605660349289938));
#9504=CARTESIAN_POINT('',(11.4,1.4227102204299,0.605660349289938));
#9505=CARTESIAN_POINT('Ctrl Pts',(11.4,1.4227102204299,0.605660349289938));
#9506=CARTESIAN_POINT('Ctrl Pts',(11.4,1.42846501637408,0.504614471147338));
#9507=CARTESIAN_POINT('Ctrl Pts',(11.4,1.43421827757761,0.403567910233218));
#9508=CARTESIAN_POINT('Ctrl Pts',(11.4,1.44570991295315,0.201681522149997));
#9509=CARTESIAN_POINT('Ctrl Pts',(11.4,1.45144836088146,0.100840510682596));
#9510=CARTESIAN_POINT('Ctrl Pts',(11.4,1.45718524058191,0.));
#9511=CARTESIAN_POINT('',(11.4,1.32241589772268,0.7));
#9512=CARTESIAN_POINT('Ctrl Pts',(11.3999999999682,1.32241589773435,0.7));
#9513=CARTESIAN_POINT('Ctrl Pts',(11.4000000023735,1.33035873561384,0.69999999792071));
#9514=CARTESIAN_POINT('Ctrl Pts',(11.3999980827719,1.33823923135401,0.699006238562837));
#9515=CARTESIAN_POINT('Ctrl Pts',(11.3999964146773,1.34591623266897,0.697118452648154));
#9516=CARTESIAN_POINT('Ctrl Pts',(11.3999954805754,1.35021521026861,0.696061327733467));
#9517=CARTESIAN_POINT('Ctrl Pts',(11.3999946303028,1.35445042327231,0.694722827332644));
#9518=CARTESIAN_POINT('Ctrl Pts',(11.3999940855437,1.35859537550353,0.6931136259882));
#9519=CARTESIAN_POINT('Ctrl Pts',(11.3999931076272,1.36603612757745,0.690224891070856));
#9520=CARTESIAN_POINT('Ctrl Pts',(11.3999932937992,1.3731074395729,0.686497549823264));
#9521=CARTESIAN_POINT('Ctrl Pts',(11.3999945206258,1.37966241828116,0.682010734965951));
#9522=CARTESIAN_POINT('Ctrl Pts',(11.3999951957832,1.38326980879772,0.679541513617388));
#9523=CARTESIAN_POINT('Ctrl Pts',(11.399996159718,1.38672054258633,0.67684140394947));
#9524=CARTESIAN_POINT('Ctrl Pts',(11.3999970106794,1.38998612808193,0.67391813047908));
#9525=CARTESIAN_POINT('Ctrl Pts',(11.399997834674,1.39314822810011,0.671087494715186));
#9526=CARTESIAN_POINT('Ctrl Pts',(11.3999985616145,1.39611771109305,0.668064564866167));
#9527=CARTESIAN_POINT('Ctrl Pts',(11.3999985600482,1.39887227052748,0.664860274403491));
#9528=CARTESIAN_POINT('Ctrl Pts',(11.3999985571253,1.40401282028653,0.65888043807832));
#9529=CARTESIAN_POINT('Ctrl Pts',(11.3999962993541,1.40840780441339,0.652270325570232));
#9530=CARTESIAN_POINT('Ctrl Pts',(11.399995545677,1.411994629421,0.6451936465425));
#9531=CARTESIAN_POINT('Ctrl Pts',(11.3999954685939,1.41236147527551,0.644469872631166));
#9532=CARTESIAN_POINT('Ctrl Pts',(11.3999954033687,1.41271982702329,0.643741199273148));
#9533=CARTESIAN_POINT('Ctrl Pts',(11.399995351278,1.41306958904162,0.643007791034547));
#9534=CARTESIAN_POINT('Ctrl Pts',(11.3999948427782,1.41648390439843,0.635848388696429));
#9535=CARTESIAN_POINT('Ctrl Pts',(11.3999960181446,1.41904356023948,0.628323447569199));
#9536=CARTESIAN_POINT('Ctrl Pts',(11.3999977140636,1.42069349507095,0.620600117586001));
#9537=CARTESIAN_POINT('Ctrl Pts',(11.3999987928026,1.4217429844709,0.615687467222433));
#9538=CARTESIAN_POINT('Ctrl Pts',(11.4,1.42242354791745,0.610693903223035));
#9539=CARTESIAN_POINT('Ctrl Pts',(11.4,1.42271022042989,0.605660349289938));
#9540=CARTESIAN_POINT('',(11.4,-1.32241589772233,0.7));
#9541=CARTESIAN_POINT('',(11.4,-0.768899768518519,0.7));
#9542=CARTESIAN_POINT('Ctrl Pts',(11.4,-1.4227102204299,0.605660349289938));
#9543=CARTESIAN_POINT('Ctrl Pts',(11.4,-1.42225988230954,0.613567634148305));
#9544=CARTESIAN_POINT('Ctrl Pts',(11.399997277834,-1.42084002197897,0.621378952482038));
#9545=CARTESIAN_POINT('Ctrl Pts',(11.3999960666067,-1.41853584574224,0.62893480307212));
#9546=CARTESIAN_POINT('Ctrl Pts',(11.3999954054252,-1.41727804822547,0.633059370437125));
#9547=CARTESIAN_POINT('Ctrl Pts',(11.399995101512,-1.41575577202439,0.637107840337094));
#9548=CARTESIAN_POINT('Ctrl Pts',(11.3999952458732,-1.4139766528271,0.641052464558972));
#9549=CARTESIAN_POINT('Ctrl Pts',(11.3999955106959,-1.41071295596475,0.648288661951321));
#9550=CARTESIAN_POINT('Ctrl Pts',(11.3999975070228,-1.40662392062869,0.655096264526915));
#9551=CARTESIAN_POINT('Ctrl Pts',(11.3999983091255,-1.40177626405188,0.661313589686923));
#9552=CARTESIAN_POINT('Ctrl Pts',(11.3999984645713,-1.40083679843637,0.66251849418371));
#9553=CARTESIAN_POINT('Ctrl Pts',(11.3999985618942,-1.3998687022723,0.663701157110503));
#9554=CARTESIAN_POINT('Ctrl Pts',(11.3999985615247,-1.39887227038638,0.664860274403572));
#9555=CARTESIAN_POINT('Ctrl Pts',(11.3999985608543,-1.39706426040285,0.666963474499402));
#9556=CARTESIAN_POINT('Ctrl Pts',(11.3999982409398,-1.39516298427334,0.668989190735049));
#9557=CARTESIAN_POINT('Ctrl Pts',(11.3999977953094,-1.39317470503404,0.670934323115149));
#9558=CARTESIAN_POINT('Ctrl Pts',(11.3999965209597,-1.38748891009577,0.67649673287249));
#9559=CARTESIAN_POINT('Ctrl Pts',(11.3999944455422,-1.38115857071774,0.681340422576046));
#9560=CARTESIAN_POINT('Ctrl Pts',(11.3999937508435,-1.37434881732181,0.685413525744465));
#9561=CARTESIAN_POINT('Ctrl Pts',(11.3999933041982,-1.36997059693002,0.688032261301096));
#9562=CARTESIAN_POINT('Ctrl Pts',(11.3999933336943,-1.3653932120823,0.69033179581025));
#9563=CARTESIAN_POINT('Ctrl Pts',(11.399993839827,-1.36065445462682,0.69228884175444));
#9564=CARTESIAN_POINT('Ctrl Pts',(11.3999946245508,-1.35330733883187,0.695323106179894));
#9565=CARTESIAN_POINT('Ctrl Pts',(11.3999965692242,-1.34565642326237,0.69750197024776));
#9566=CARTESIAN_POINT('Ctrl Pts',(11.3999981510416,-1.33784990929195,0.698756936804364));
#9567=CARTESIAN_POINT('Ctrl Pts',(11.399999182603,-1.33275899381189,0.699575346749464));
#9568=CARTESIAN_POINT('Ctrl Pts',(11.4000000015384,-1.32760128986121,0.699999998642559));
#9569=CARTESIAN_POINT('Ctrl Pts',(11.3999999999682,-1.32241589773435,0.7));
#9570=CARTESIAN_POINT('Ctrl Pts',(11.227882892666,-1.47337141465794,-0.000640335460849732));
#9571=CARTESIAN_POINT('Ctrl Pts',(11.218588765022,-1.46278323638644,0.201451598614313));
#9572=CARTESIAN_POINT('Ctrl Pts',(11.2092944683555,-1.45219508216535,0.40354352620373));
#9573=CARTESIAN_POINT('Ctrl Pts',(11.2000000000001,-1.44160695250309,0.60563544721184));
#9574=CARTESIAN_POINT('Ctrl Pts',(10.1843397214697,-1.57034855377304,-0.000384310983874139));
#9575=CARTESIAN_POINT('Ctrl Pts',(10.1768953195658,-1.55975965902304,0.201708049868595));
#9576=CARTESIAN_POINT('Ctrl Pts',(10.1694507716805,-1.54917076711515,0.403800406245857));
#9577=CARTESIAN_POINT('Ctrl Pts',(10.1620060668616,-1.53858190981164,0.605892758286982));
#9578=CARTESIAN_POINT('Ctrl Pts',(9.14170648965309,-1.65016851777514,-0.000148134864058495));
#9579=CARTESIAN_POINT('Ctrl Pts',(9.13611341817177,-1.63957870617509,0.201944615677573));
#9580=CARTESIAN_POINT('Ctrl Pts',(9.13052023035058,-1.6289888900612,0.404037363603497));
#9581=CARTESIAN_POINT('Ctrl Pts',(9.124926910836,-1.6183991014662,0.606130109186173));
#9582=CARTESIAN_POINT('Ctrl Pts',(8.1,-1.69866351109718,1.00613961606655E-16));
#9583=CARTESIAN_POINT('Ctrl Pts',(8.09625995443094,-1.68807302815665,0.202092993803311));
#9584=CARTESIAN_POINT('Ctrl Pts',(8.09251982249141,-1.67748255132318,0.404185986335255));
#9585=CARTESIAN_POINT('Ctrl Pts',(8.08877960280056,-1.66689208072706,0.606278977577217));
#9586=CARTESIAN_POINT('Ctrl Pts',(8.1,-1.66641703131627,0.605314487869832));
#9587=CARTESIAN_POINT('Ctrl Pts',(9.13548525483003,-1.617718421277,0.605389190939432));
#9588=CARTESIAN_POINT('Ctrl Pts',(10.168822041161,-1.53796707615457,0.605507632815633));
#9589=CARTESIAN_POINT('Ctrl Pts',(11.2000000000893,-1.44160695345912,0.605635447210802));
#9590=CARTESIAN_POINT('Ctrl Pts',(11.7095939787209,-1.42740645209206,-7.69249563980189E-5));
#9591=CARTESIAN_POINT('Ctrl Pts',(11.6994545874061,-1.41682738380082,0.201847033339061));
#9592=CARTESIAN_POINT('Ctrl Pts',(11.6893150192885,-1.40624834198077,0.403770984173611));
#9593=CARTESIAN_POINT('Ctrl Pts',(11.6791752715866,-1.39566932719028,0.605694927437301));
#9594=CARTESIAN_POINT('Ctrl Pts',(11.6063871276792,-1.43748358609578,-5.11721697277706E-5));
#9595=CARTESIAN_POINT('Ctrl Pts',(11.596430427176,-1.42690445239132,0.201872829148883));
#9596=CARTESIAN_POINT('Ctrl Pts',(11.5864735514701,-1.41632534465399,0.403796823219986));
#9597=CARTESIAN_POINT('Ctrl Pts',(11.5765164978042,-1.40574626343445,0.605720809936841));
#9598=CARTESIAN_POINT('Ctrl Pts',(11.5031891278894,-1.4474144288224,-2.55082377288765E-5));
#9599=CARTESIAN_POINT('Ctrl Pts',(11.4934151336386,-1.43683522760458,0.201898535909597));
#9600=CARTESIAN_POINT('Ctrl Pts',(11.4836409658656,-1.42625605183456,0.40382257302165));
#9601=CARTESIAN_POINT('Ctrl Pts',(11.4738666218385,-1.41567690205216,0.605746602994839));
#9602=CARTESIAN_POINT('Ctrl Pts',(11.4,-1.45718524058191,-5.20417042793042E-18));
#9603=CARTESIAN_POINT('Ctrl Pts',(11.3904087275488,-1.44660597001679,0.201924086674796));
#9604=CARTESIAN_POINT('Ctrl Pts',(11.3808172833376,-1.43602672436683,0.403848166524883));
#9605=CARTESIAN_POINT('Ctrl Pts',(11.3712256646606,-1.42544750415802,0.605772239449758));
#9606=CARTESIAN_POINT('',(11.6778970386953,-1.39579479040469,0.605695249702977));
#9607=CARTESIAN_POINT('Ctrl Pts',(11.4,-1.4227102204299,0.605660349289938));
#9608=CARTESIAN_POINT('Ctrl Pts',(11.4926474653491,-1.41386220753305,0.605671932550561));
#9609=CARTESIAN_POINT('Ctrl Pts',(11.585279512325,-1.40488700096013,0.605683574233495));
#9610=CARTESIAN_POINT('Ctrl Pts',(11.6778970386953,-1.39579479040469,0.605695249702977));
#9611=CARTESIAN_POINT('Ctrl Pts',(11.6778970386953,-1.39579479040469,0.605695249702977));
#9612=CARTESIAN_POINT('Ctrl Pts',(11.6884613130147,-1.40633044792991,0.403796817797553));
#9613=CARTESIAN_POINT('Ctrl Pts',(11.6990256725537,-1.41686632615463,0.201898401304098));
#9614=CARTESIAN_POINT('Ctrl Pts',(11.7095901160181,-1.42740242188993,5.19332840620557E-17));
#9615=CARTESIAN_POINT('Ctrl Pts',(11.2,-1.34133050917871,0.7));
#9616=CARTESIAN_POINT('Ctrl Pts',(10.1668086441106,-1.43797263608903,0.7));
#9617=CARTESIAN_POINT('Ctrl Pts',(9.13190264019122,-1.51792184128158,0.7));
#9618=CARTESIAN_POINT('Ctrl Pts',(8.09530923905977,-1.56666858280461,0.7));
#9619=CARTESIAN_POINT('Ctrl Pts',(11.2026864299662,-1.37005086445236,0.7));
#9620=CARTESIAN_POINT('Ctrl Pts',(10.1691860218014,-1.46674693471719,0.700000910790016));
#9621=CARTESIAN_POINT('Ctrl Pts',(9.13384227773975,-1.54675516497,0.699999464833944));
#9622=CARTESIAN_POINT('Ctrl Pts',(8.09666712422266,-1.59554384206015,0.700000000000001));
#9623=CARTESIAN_POINT('Ctrl Pts',(11.2073428085028,-1.4198317437391,0.676744232988519));
#9624=CARTESIAN_POINT('Ctrl Pts',(10.1733099382853,-1.51661799675652,0.676702307311825));
#9625=CARTESIAN_POINT('Ctrl Pts',(9.13719745543551,-1.59672983278297,0.676663906627884));
#9626=CARTESIAN_POINT('Ctrl Pts',(8.09902054834098,-1.64558911349573,0.676639354455264));
#9627=CARTESIAN_POINT('Ctrl Pts',(11.2091847227485,-1.43952346553595,0.627236497176141));
#9628=CARTESIAN_POINT('Ctrl Pts',(10.1749352046592,-1.53629892039422,0.62712791425818));
#9629=CARTESIAN_POINT('Ctrl Pts',(9.13852107143019,-1.61640633519008,0.627027713743691));
#9630=CARTESIAN_POINT('Ctrl Pts',(8.0999458765183,-1.66526610220338,0.626964226563296));
#9631=CARTESIAN_POINT('Ctrl Pts',(11.209298290232,-1.4407376041935,0.605636599993194));
#9632=CARTESIAN_POINT('Ctrl Pts',(10.1750338985877,-1.53748737250229,0.605508345221004));
#9633=CARTESIAN_POINT('Ctrl Pts',(9.13859765097935,-1.61757204607208,0.605389415477198));
#9634=CARTESIAN_POINT('Ctrl Pts',(8.1,-1.66641703131627,0.605314487869832));
#9635=CARTESIAN_POINT('Ctrl Pts',(11.2,-1.34133050917871,0.7));
#9636=CARTESIAN_POINT('Ctrl Pts',(10.16836710286,-1.43782686176815,0.7));
#9637=CARTESIAN_POINT('Ctrl Pts',(9.13502472651537,-1.51768061363633,0.7));
#9638=CARTESIAN_POINT('Ctrl Pts',(8.09999999865516,-1.56644778212326,0.7));
#9639=CARTESIAN_POINT('Ctrl Pts',(11.6681436286308,-1.2964346619681,0.7));
#9640=CARTESIAN_POINT('Ctrl Pts',(11.5756099286391,-1.3055179747114,0.7));
#9641=CARTESIAN_POINT('Ctrl Pts',(11.4830653488871,-1.31448403714215,0.7));
#9642=CARTESIAN_POINT('Ctrl Pts',(11.3905090053564,-1.32332268868375,0.7));
#9643=CARTESIAN_POINT('Ctrl Pts',(11.6709605510772,-1.32513126902304,0.700000000000001));
#9644=CARTESIAN_POINT('Ctrl Pts',(11.5784027531871,-1.33421922733773,0.700000082825348));
#9645=CARTESIAN_POINT('Ctrl Pts',(11.4858332859074,-1.34318985044544,0.699999917777441));
#9646=CARTESIAN_POINT('Ctrl Pts',(11.3932507170007,-1.35203326785046,0.7));
#9647=CARTESIAN_POINT('Ctrl Pts',(11.6758431636759,-1.37487151491717,0.67676311428296));
#9648=CARTESIAN_POINT('Ctrl Pts',(11.583243842395,-1.38396722707511,0.676759299309384));
#9649=CARTESIAN_POINT('Ctrl Pts',(11.4906306781253,-1.39294591144353,0.676755553516685));
#9650=CARTESIAN_POINT('Ctrl Pts',(11.3980029235659,-1.40179729139028,0.67675176769038));
#9651=CARTESIAN_POINT('Ctrl Pts',(11.6777767156198,-1.39456903283364,0.627286048421068));
#9652=CARTESIAN_POINT('Ctrl Pts',(11.5851604051362,-1.40366358810601,0.627276165220861));
#9653=CARTESIAN_POINT('Ctrl Pts',(11.4925297866457,-1.41264104586547,0.627266369072496));
#9654=CARTESIAN_POINT('Ctrl Pts',(11.3998836071583,-1.4214913811319,0.627256563056779));
#9655=CARTESIAN_POINT('Ctrl Pts',(11.6778970386953,-1.39579479040469,0.605695249702977));
#9656=CARTESIAN_POINT('Ctrl Pts',(11.585279512325,-1.40488700096013,0.605683574233495));
#9657=CARTESIAN_POINT('Ctrl Pts',(11.4926474653491,-1.41386220753305,0.605671932550561));
#9658=CARTESIAN_POINT('Ctrl Pts',(11.4,-1.4227102204299,0.605660349289938));
#9659=CARTESIAN_POINT('',(11.6681436286308,-1.2964346619681,0.7));
#9660=CARTESIAN_POINT('Ctrl Pts',(11.6681436286308,-1.2964346619681,0.7));
#9661=CARTESIAN_POINT('Ctrl Pts',(11.5787728332608,-1.30520749699507,0.7));
#9662=CARTESIAN_POINT('Ctrl Pts',(11.4893918891838,-1.31387096021207,0.7));
#9663=CARTESIAN_POINT('Ctrl Pts',(11.3999999999682,-1.32241589773435,0.7));
#9664=CARTESIAN_POINT('Origin',(11.6681436286308,-1.2964346619681,0.6));
#9665=CARTESIAN_POINT('Origin',(6.08012166120517,1.06778195214465E-16,0.7));
#9666=CARTESIAN_POINT('Ctrl Pts',(8.0999999986552,1.56644778212326,0.7));
#9667=CARTESIAN_POINT('Ctrl Pts',(9.13502472651542,1.51768061363633,0.7));
#9668=CARTESIAN_POINT('Ctrl Pts',(10.16836710286,1.43782686176815,0.7));
#9669=CARTESIAN_POINT('Ctrl Pts',(11.2,1.34133050917871,0.7));
#9670=CARTESIAN_POINT('Origin',(6.08012166120517,1.06778195214465E-16,0.7));
#9671=CARTESIAN_POINT('',(11.6681436286308,1.2964346619681,0.7));
#9672=CARTESIAN_POINT('Ctrl Pts',(11.3999999999682,1.32241589773435,0.7));
#9673=CARTESIAN_POINT('Ctrl Pts',(11.4893918891837,1.31387096021208,0.7));
#9674=CARTESIAN_POINT('Ctrl Pts',(11.5787728332608,1.30520749699508,0.7));
#9675=CARTESIAN_POINT('Ctrl Pts',(11.6681436286308,1.2964346619681,0.7));
#9676=CARTESIAN_POINT('',(11.6681436286308,0.8,0.7));
#9677=CARTESIAN_POINT('Ctrl Pts',(8.09530923905978,1.56666858280461,0.7));
#9678=CARTESIAN_POINT('Ctrl Pts',(9.13190264019124,1.51792184128158,0.7));
#9679=CARTESIAN_POINT('Ctrl Pts',(10.1668086441106,1.43797263608903,0.7));
#9680=CARTESIAN_POINT('Ctrl Pts',(11.2,1.34133050917871,0.7));
#9681=CARTESIAN_POINT('Ctrl Pts',(8.09666712422266,1.59554384206015,0.700000000000001));
#9682=CARTESIAN_POINT('Ctrl Pts',(9.13384227773977,1.54675516497,0.699999464833944));
#9683=CARTESIAN_POINT('Ctrl Pts',(10.1691860218013,1.46674693471719,0.700000910790016));
#9684=CARTESIAN_POINT('Ctrl Pts',(11.2026864299662,1.37005086445236,0.7));
#9685=CARTESIAN_POINT('Ctrl Pts',(8.09902054834099,1.64558911349573,0.676639354455264));
#9686=CARTESIAN_POINT('Ctrl Pts',(9.13719745543553,1.59672983278297,0.676663906627884));
#9687=CARTESIAN_POINT('Ctrl Pts',(10.1733099382853,1.51661799675652,0.676702307311825));
#9688=CARTESIAN_POINT('Ctrl Pts',(11.2073428085028,1.4198317437391,0.676744232988519));
#9689=CARTESIAN_POINT('Ctrl Pts',(8.0999458765183,1.66526610220338,0.626964226563296));
#9690=CARTESIAN_POINT('Ctrl Pts',(9.1385210714302,1.61640633519008,0.627027713743691));
#9691=CARTESIAN_POINT('Ctrl Pts',(10.1749352046592,1.53629892039423,0.62712791425818));
#9692=CARTESIAN_POINT('Ctrl Pts',(11.2091847227485,1.43952346553595,0.627236497176141));
#9693=CARTESIAN_POINT('Ctrl Pts',(8.1,1.66641703131627,0.605314487869832));
#9694=CARTESIAN_POINT('Ctrl Pts',(9.13859765097937,1.61757204607208,0.605389415477198));
#9695=CARTESIAN_POINT('Ctrl Pts',(10.1750338985877,1.53748737250229,0.605508345221004));
#9696=CARTESIAN_POINT('Ctrl Pts',(11.209298290232,1.4407376041935,0.605636599993194));
#9697=CARTESIAN_POINT('Ctrl Pts',(11.2000000000893,1.44160695345912,0.605635447210802));
#9698=CARTESIAN_POINT('Ctrl Pts',(10.168822041161,1.53796707615457,0.605507632815633));
#9699=CARTESIAN_POINT('Ctrl Pts',(9.13548525483005,1.617718421277,0.605389190939432));
#9700=CARTESIAN_POINT('Ctrl Pts',(8.1,1.66641703131627,0.605314487869832));
#9701=CARTESIAN_POINT('Ctrl Pts',(8.1,1.69866351109859,-2.6441702993818E-11));
#9702=CARTESIAN_POINT('Ctrl Pts',(8.09625995443078,1.68807302815759,0.202092993785684));
#9703=CARTESIAN_POINT('Ctrl Pts',(8.09251982249108,1.67748255132366,0.404185986326441));
#9704=CARTESIAN_POINT('Ctrl Pts',(8.08877960280008,1.66689208072708,0.606278977577217));
#9705=CARTESIAN_POINT('Ctrl Pts',(9.14170648965349,1.65016851777655,-0.00014813489050026));
#9706=CARTESIAN_POINT('Ctrl Pts',(9.13611341817193,1.63957870617604,0.201944615659945));
#9707=CARTESIAN_POINT('Ctrl Pts',(9.1305202303505,1.62898889006169,0.404037363594684));
#9708=CARTESIAN_POINT('Ctrl Pts',(9.12492691083567,1.61839910146622,0.606130109186173));
#9709=CARTESIAN_POINT('Ctrl Pts',(10.1843397214705,1.57034855377444,-0.000384311010315772));
#9710=CARTESIAN_POINT('Ctrl Pts',(10.1768953195662,1.55975965902398,0.201708049850968));
#9711=CARTESIAN_POINT('Ctrl Pts',(10.1694507716807,1.54917076711562,0.403800406237042));
#9712=CARTESIAN_POINT('Ctrl Pts',(10.1620060668615,1.53858190981166,0.605892758286982));
#9713=CARTESIAN_POINT('Ctrl Pts',(11.2278828926672,1.47337141465933,-0.000640335487291374));
#9714=CARTESIAN_POINT('Ctrl Pts',(11.2185887650228,1.46278323638736,0.201451598596686));
#9715=CARTESIAN_POINT('Ctrl Pts',(11.2092944683559,1.45219508216582,0.403543526194916));
#9716=CARTESIAN_POINT('Ctrl Pts',(11.2000000000001,1.44160695250309,0.60563544721184));
#9717=CARTESIAN_POINT('Ctrl Pts',(11.4,1.45718524058191,-1.37043154602168E-16));
#9718=CARTESIAN_POINT('Ctrl Pts',(11.3904087275488,1.44660597001679,0.201924086674796));
#9719=CARTESIAN_POINT('Ctrl Pts',(11.3808172833376,1.43602672436683,0.403848166524884));
#9720=CARTESIAN_POINT('Ctrl Pts',(11.3712256646606,1.42544750415802,0.605772239449759));
#9721=CARTESIAN_POINT('Ctrl Pts',(11.5031891278894,1.4474144288224,-2.55082377290153E-5));
#9722=CARTESIAN_POINT('Ctrl Pts',(11.4934151336386,1.43683522760458,0.201898535909598));
#9723=CARTESIAN_POINT('Ctrl Pts',(11.4836409658656,1.42625605183455,0.40382257302165));
#9724=CARTESIAN_POINT('Ctrl Pts',(11.4738666218385,1.41567690205216,0.605746602994839));
#9725=CARTESIAN_POINT('Ctrl Pts',(11.6063871276792,1.43748358609579,-5.1172169727805E-5));
#9726=CARTESIAN_POINT('Ctrl Pts',(11.596430427176,1.42690445239132,0.201872829148883));
#9727=CARTESIAN_POINT('Ctrl Pts',(11.5864735514701,1.41632534465399,0.403796823219986));
#9728=CARTESIAN_POINT('Ctrl Pts',(11.5765164978042,1.40574626343445,0.605720809936842));
#9729=CARTESIAN_POINT('Ctrl Pts',(11.7095939787209,1.42740645209206,-7.69249563980588E-5));
#9730=CARTESIAN_POINT('Ctrl Pts',(11.6994545874061,1.41682738380082,0.201847033339061));
#9731=CARTESIAN_POINT('Ctrl Pts',(11.6893150192885,1.40624834198077,0.403770984173611));
#9732=CARTESIAN_POINT('Ctrl Pts',(11.6791752715866,1.39566932719028,0.605694927437301));
#9733=CARTESIAN_POINT('',(11.6778970386953,1.39579479040469,0.605695249702977));
#9734=CARTESIAN_POINT('Ctrl Pts',(11.7095901160181,1.42740242188993,2.01986864734049E-16));
#9735=CARTESIAN_POINT('Ctrl Pts',(11.6990256725537,1.41686632615463,0.201898401304098));
#9736=CARTESIAN_POINT('Ctrl Pts',(11.6884613130147,1.40633044792991,0.403796817797553));
#9737=CARTESIAN_POINT('Ctrl Pts',(11.6778970386953,1.39579479040469,0.605695249702978));
#9738=CARTESIAN_POINT('Ctrl Pts',(11.6778970386953,1.39579479040469,0.605695249702977));
#9739=CARTESIAN_POINT('Ctrl Pts',(11.585279512325,1.40488700096013,0.605683574233495));
#9740=CARTESIAN_POINT('Ctrl Pts',(11.4926474653491,1.41386220753305,0.605671932550561));
#9741=CARTESIAN_POINT('Ctrl Pts',(11.4,1.4227102204299,0.605660349289938));
#9742=CARTESIAN_POINT('Origin',(7.9,1.7737037037037,0.));
#9743=CARTESIAN_POINT('',(7.9,-1.67543132363858,0.605300614462415));
#9744=CARTESIAN_POINT('Ctrl Pts',(7.9,-1.67543132363858,0.605300614462415));
#9745=CARTESIAN_POINT('Ctrl Pts',(7.9,-1.68078196203297,0.504592238472094));
#9746=CARTESIAN_POINT('Ctrl Pts',(7.9,-1.68613236521525,0.403883028813119));
#9747=CARTESIAN_POINT('Ctrl Pts',(7.9,-1.69685110017509,0.202116711316755));
#9748=CARTESIAN_POINT('Ctrl Pts',(7.9,-1.70221951791351,0.10105794916591));
#9749=CARTESIAN_POINT('Ctrl Pts',(7.9,-1.70758761671949,0.));
#9750=CARTESIAN_POINT('',(7.9,-1.57547905376932,0.7));
#9751=CARTESIAN_POINT('Ctrl Pts',(7.9,-1.57547905376882,0.7));
#9752=CARTESIAN_POINT('Ctrl Pts',(7.9,-1.58339333479856,0.700000000000001));
#9753=CARTESIAN_POINT('Ctrl Pts',(7.89999913038498,-1.59124411312484,0.699006032637452));
#9754=CARTESIAN_POINT('Ctrl Pts',(7.89999837104309,-1.59889106951376,0.697118831203047));
#9755=CARTESIAN_POINT('Ctrl Pts',(7.89999794343345,-1.6031973145812,0.696056087876834));
#9756=CARTESIAN_POINT('Ctrl Pts',(7.89999755365678,-1.60743898057435,0.694709047589066));
#9757=CARTESIAN_POINT('Ctrl Pts',(7.89999730661842,-1.61158931211603,0.693088720937666));
#9758=CARTESIAN_POINT('Ctrl Pts',(7.89999686465941,-1.6190143793929,0.690189908089508));
#9759=CARTESIAN_POINT('Ctrl Pts',(7.89999696143539,-1.626066934352,0.686450944759811));
#9760=CARTESIAN_POINT('Ctrl Pts',(7.89999752554231,-1.63260082031789,0.681953255064161));
#9761=CARTESIAN_POINT('Ctrl Pts',(7.89999783650325,-1.63620259020663,0.679473927540052));
#9762=CARTESIAN_POINT('Ctrl Pts',(7.89999827825103,-1.63964648551863,0.676763160200805));
#9763=CARTESIAN_POINT('Ctrl Pts',(7.89999867021687,-1.64290407802379,0.673829034208746));
#9764=CARTESIAN_POINT('Ctrl Pts',(7.89999905115172,-1.64606999298761,0.670977482527793));
#9765=CARTESIAN_POINT('Ctrl Pts',(7.89999938859403,-1.64904076201529,0.667932171841817));
#9766=CARTESIAN_POINT('Ctrl Pts',(7.89999938783828,-1.6517939440564,0.66470449824639));
#9767=CARTESIAN_POINT('Ctrl Pts',(7.89999938643498,-1.65690611124346,0.658711285012161));
#9768=CARTESIAN_POINT('Ctrl Pts',(7.89999834643869,-1.661271022418,0.652090721578155));
#9769=CARTESIAN_POINT('Ctrl Pts',(7.89999799057748,-1.66482884904143,0.645008203309728));
#9770=CARTESIAN_POINT('Ctrl Pts',(7.89999795399159,-1.66519462718329,0.644280053614395));
#9771=CARTESIAN_POINT('Ctrl Pts',(7.89999792287445,-1.66555183396469,0.643547001244109));
#9772=CARTESIAN_POINT('Ctrl Pts',(7.89999789784292,-1.66590037542058,0.642809214685104));
#9773=CARTESIAN_POINT('Ctrl Pts',(7.89999765441981,-1.66928982250308,0.635634491398386));
#9774=CARTESIAN_POINT('Ctrl Pts',(7.89999817709027,-1.67182454272713,0.628096763436417));
#9775=CARTESIAN_POINT('Ctrl Pts',(7.8999989464625,-1.67345106343068,0.620364350320046));
#9776=CARTESIAN_POINT('Ctrl Pts',(7.89999943944948,-1.67449328136075,0.615409688768565));
#9777=CARTESIAN_POINT('Ctrl Pts',(7.89999999630063,-1.67516175160204,0.610374426093907));
#9778=CARTESIAN_POINT('Ctrl Pts',(7.89999999769359,-1.67543132314592,0.605300614465834));
#9779=CARTESIAN_POINT('',(7.9,1.57547905376882,0.7));
#9780=CARTESIAN_POINT('',(7.9,0.886851851851852,0.7));
#9781=CARTESIAN_POINT('',(7.9,1.67543132363858,0.605300614462415));
#9782=CARTESIAN_POINT('Ctrl Pts',(7.89999999769359,1.67543132314592,0.605300614465834));
#9783=CARTESIAN_POINT('Ctrl Pts',(7.89999999552123,1.67501091691767,0.613213400729193));
#9784=CARTESIAN_POINT('Ctrl Pts',(7.89999875799714,1.67362284400845,0.621034919585595));
#9785=CARTESIAN_POINT('Ctrl Pts',(7.89999821041927,1.67135120200026,0.628604813990272));
#9786=CARTESIAN_POINT('Ctrl Pts',(7.89999790518813,1.67008494211401,0.632824428521627));
#9787=CARTESIAN_POINT('Ctrl Pts',(7.89999777089825,1.66854314417455,0.636965893954691));
#9788=CARTESIAN_POINT('Ctrl Pts',(7.89999784944871,1.66673368022774,0.640999456224326));
#9789=CARTESIAN_POINT('Ctrl Pts',(7.89999799035603,1.66348778281681,0.648235040746992));
#9790=CARTESIAN_POINT('Ctrl Pts',(7.8999989183875,1.65941887886545,0.655045206964536));
#9791=CARTESIAN_POINT('Ctrl Pts',(7.89999927807636,1.65459101651367,0.661266862646797));
#9792=CARTESIAN_POINT('Ctrl Pts',(7.89999934554656,1.65368540929837,0.662433916689859));
#9793=CARTESIAN_POINT('Ctrl Pts',(7.89999938740919,1.65275296801062,0.663580193269421));
#9794=CARTESIAN_POINT('Ctrl Pts',(7.89999938728957,1.65179394408007,0.664704498246374));
#9795=CARTESIAN_POINT('Ctrl Pts',(7.89999938705343,1.64990069294102,0.666924037937161));
#9796=CARTESIAN_POINT('Ctrl Pts',(7.89999922461202,1.64790387543569,0.669057997255949));
#9797=CARTESIAN_POINT('Ctrl Pts',(7.89999900301747,1.64581073954063,0.671102663899023));
#9798=CARTESIAN_POINT('Ctrl Pts',(7.89999840121276,1.64012621790684,0.676655553128015));
#9799=CARTESIAN_POINT('Ctrl Pts',(7.89999746538644,1.63379824275617,0.681490110487894));
#9800=CARTESIAN_POINT('Ctrl Pts',(7.89999715581736,1.6269906793715,0.685552192443336));
#9801=CARTESIAN_POINT('Ctrl Pts',(7.89999695885968,1.62265949106942,0.688136618155352));
#9802=CARTESIAN_POINT('Ctrl Pts',(7.89999697413705,1.61813320929371,0.690407672840119));
#9803=CARTESIAN_POINT('Ctrl Pts',(7.89999720528031,1.61344832872307,0.692342105328139));
#9804=CARTESIAN_POINT('Ctrl Pts',(7.89999756646959,1.60612763680413,0.69536488980882));
#9805=CARTESIAN_POINT('Ctrl Pts',(7.89999845750109,1.59850458633822,0.69753330980446));
#9806=CARTESIAN_POINT('Ctrl Pts',(7.89999917312139,1.59072625322659,0.698777780766876));
#9807=CARTESIAN_POINT('Ctrl Pts',(7.8999996358458,1.58569673594883,0.699582463224842));
#9808=CARTESIAN_POINT('Ctrl Pts',(7.9,1.58060170040825,0.7));
#9809=CARTESIAN_POINT('Ctrl Pts',(7.9,1.57547905376882,0.7));
#9810=CARTESIAN_POINT('Ctrl Pts',(7.9,1.70758761671949,0.));
#9811=CARTESIAN_POINT('Ctrl Pts',(7.9,1.70221949782947,0.101058327261027));
#9812=CARTESIAN_POINT('Ctrl Pts',(7.9,1.69685105999395,0.202117467714));
#9813=CARTESIAN_POINT('Ctrl Pts',(7.9,1.68613232500772,0.403883785628764));
#9814=CARTESIAN_POINT('Ctrl Pts',(7.9,1.6807819419292,0.504592616860323));
#9815=CARTESIAN_POINT('Ctrl Pts',(7.9,1.67543132363858,0.605300614462415));
#9816=CARTESIAN_POINT('Ctrl Pts',(7.91019312999368,-1.70715886092982,-0.000134090250286965));
#9817=CARTESIAN_POINT('Ctrl Pts',(7.90679525219671,-1.69658223918655,0.201692187253877));
#9818=CARTESIAN_POINT('Ctrl Pts',(7.90339729501941,-1.68600562260833,0.40351846369823));
#9819=CARTESIAN_POINT('Ctrl Pts',(7.89999925719352,-1.67542901130525,0.605344739067286));
#9820=CARTESIAN_POINT('Ctrl Pts',(6.63535348802246,-1.76179300886274,3.38453142643293E-5));
#9821=CARTESIAN_POINT('Ctrl Pts',(6.63422081661327,-1.7512156246026,0.201860399405878));
#9822=CARTESIAN_POINT('Ctrl Pts',(6.6330881724013,-1.74063821514668,0.403686949685767));
#9823=CARTESIAN_POINT('Ctrl Pts',(6.63195543348167,-1.7300608292057,0.605513504373875));
#9824=CARTESIAN_POINT('Ctrl Pts',(5.36191629096386,-1.76821426310706,6.25694230841134E-5));
#9825=CARTESIAN_POINT('Ctrl Pts',(5.36305144950513,-1.75763653444312,0.201889164820622));
#9826=CARTESIAN_POINT('Ctrl Pts',(5.36418670601529,-1.74705878452761,0.403715755186214));
#9827=CARTESIAN_POINT('Ctrl Pts',(5.36532191986746,-1.73648104871457,0.605542351516859));
#9828=CARTESIAN_POINT('Ctrl Pts',(4.08978435919194,-1.70060618495018,-0.000163379468877527));
#9829=CARTESIAN_POINT('Ctrl Pts',(4.09318947412453,-1.69002991101751,0.201662855819258));
#9830=CARTESIAN_POINT('Ctrl Pts',(4.09659468720556,-1.67945364498778,0.403489089874722));
#9831=CARTESIAN_POINT('Ctrl Pts',(4.1,-1.66887738702936,0.605315322680078));
#9832=CARTESIAN_POINT('Ctrl Pts',(4.10000000006189,-1.66887738587128,0.605315322687833));
#9833=CARTESIAN_POINT('Ctrl Pts',(5.36600428635239,-1.73653511802878,0.605201749988751));
#9834=CARTESIAN_POINT('Ctrl Pts',(6.63469107356441,-1.72995836404769,0.605216415547347));
#9835=CARTESIAN_POINT('Ctrl Pts',(7.89999999997453,-1.67543132304763,0.605300614465986));
#9836=CARTESIAN_POINT('Ctrl Pts',(7.9,-1.57547905376882,0.7));
#9837=CARTESIAN_POINT('Ctrl Pts',(6.63400208894818,-1.63014048526579,0.7));
#9838=CARTESIAN_POINT('Ctrl Pts',(5.36531976402288,-1.63670020240541,0.7));
#9839=CARTESIAN_POINT('Ctrl Pts',(4.09999999999999,-1.56887583540973,0.7));
#9840=CARTESIAN_POINT('Ctrl Pts',(7.9012470621039,-1.60436190544783,0.700000000000001));
#9841=CARTESIAN_POINT('Ctrl Pts',(6.6345175325877,-1.65907137725265,0.700000604190856));
#9842=CARTESIAN_POINT('Ctrl Pts',(5.36490325870521,-1.66564852467601,0.700000815814724));
#9843=CARTESIAN_POINT('Ctrl Pts',(4.09845273665223,-1.59774131518914,0.699999999999999));
#9844=CARTESIAN_POINT('Ctrl Pts',(7.90340849276168,-1.6544221878571,0.676636720659303));
#9845=CARTESIAN_POINT('Ctrl Pts',(6.63541917043928,-1.70921256696412,0.676609005714152));
#9846=CARTESIAN_POINT('Ctrl Pts',(5.36416860778507,-1.71581908642683,0.67660414986632));
#9847=CARTESIAN_POINT('Ctrl Pts',(4.09577098158984,-1.64777167791894,0.676641578059328));
#9848=CARTESIAN_POINT('Ctrl Pts',(7.90425799286387,-1.67409721877663,0.626952737571144));
#9849=CARTESIAN_POINT('Ctrl Pts',(6.63576820027036,-1.72888861107585,0.626881076846221));
#9850=CARTESIAN_POINT('Ctrl Pts',(5.36388821219926,-1.73550154452763,0.626868555890157));
#9851=CARTESIAN_POINT('Ctrl Pts',(4.09471668402893,-1.66744047248441,0.626965338598652));
#9852=CARTESIAN_POINT('Ctrl Pts',(7.90430757201307,-1.67524550738887,0.605300901379154));
#9853=CARTESIAN_POINT('Ctrl Pts',(6.63578978311492,-1.73002023206136,0.605216330280387));
#9854=CARTESIAN_POINT('Ctrl Pts',(5.3638700255334,-1.7366305488338,0.605201579557148));
#9855=CARTESIAN_POINT('Ctrl Pts',(4.09465499692593,-1.6685912965035,0.605315802949303));
#9856=CARTESIAN_POINT('Ctrl Pts',(7.9,-1.57547905376882,0.7));
#9857=CARTESIAN_POINT('Ctrl Pts',(6.63400208894818,-1.63014048526579,0.7));
#9858=CARTESIAN_POINT('Ctrl Pts',(5.36531976402288,-1.63670020240541,0.7));
#9859=CARTESIAN_POINT('Ctrl Pts',(4.09999999999999,-1.56887583540973,0.7));
#9860=CARTESIAN_POINT('Origin',(6.08012166120517,1.06778195214465E-16,0.7));
#9861=CARTESIAN_POINT('Ctrl Pts',(4.1,1.56887583540973,0.7));
#9862=CARTESIAN_POINT('Ctrl Pts',(5.36531976402291,1.63670020240541,0.7));
#9863=CARTESIAN_POINT('Ctrl Pts',(6.63400208894819,1.63014048526579,0.7));
#9864=CARTESIAN_POINT('Ctrl Pts',(7.9,1.57547905376882,0.7));
#9865=CARTESIAN_POINT('Ctrl Pts',(4.1,1.56887583540973,0.7));
#9866=CARTESIAN_POINT('Ctrl Pts',(5.36531976402291,1.63670020240541,0.7));
#9867=CARTESIAN_POINT('Ctrl Pts',(6.63400208894819,1.63014048526579,0.7));
#9868=CARTESIAN_POINT('Ctrl Pts',(7.9,1.57547905376882,0.7));
#9869=CARTESIAN_POINT('Ctrl Pts',(4.09845273665224,1.59774131518914,0.699999999999999));
#9870=CARTESIAN_POINT('Ctrl Pts',(5.36490325870523,1.66564852467601,0.700000815814725));
#9871=CARTESIAN_POINT('Ctrl Pts',(6.6345175325877,1.65907137725265,0.700000604190856));
#9872=CARTESIAN_POINT('Ctrl Pts',(7.9012470621039,1.60436190544783,0.700000000000001));
#9873=CARTESIAN_POINT('Ctrl Pts',(4.09577098158985,1.64777167791894,0.676641578059328));
#9874=CARTESIAN_POINT('Ctrl Pts',(5.36416860778509,1.71581908642683,0.67660414986632));
#9875=CARTESIAN_POINT('Ctrl Pts',(6.6354191704393,1.70921256696412,0.676609005714152));
#9876=CARTESIAN_POINT('Ctrl Pts',(7.90340849276168,1.6544221878571,0.676636720659302));
#9877=CARTESIAN_POINT('Ctrl Pts',(4.09471668402895,1.66744047248441,0.626965338598652));
#9878=CARTESIAN_POINT('Ctrl Pts',(5.36388821219928,1.73550154452763,0.626868555890157));
#9879=CARTESIAN_POINT('Ctrl Pts',(6.63576820027036,1.72888861107585,0.626881076846221));
#9880=CARTESIAN_POINT('Ctrl Pts',(7.90425799286387,1.67409721877663,0.626952737571144));
#9881=CARTESIAN_POINT('Ctrl Pts',(4.09465499692594,1.6685912965035,0.605315802949303));
#9882=CARTESIAN_POINT('Ctrl Pts',(5.36387002553342,1.7366305488338,0.605201579557148));
#9883=CARTESIAN_POINT('Ctrl Pts',(6.63578978311492,1.73002023206136,0.605216330280387));
#9884=CARTESIAN_POINT('Ctrl Pts',(7.90430757201307,1.67524550738887,0.605300901379154));
#9885=CARTESIAN_POINT('Ctrl Pts',(7.89999999997454,1.67543132304763,0.605300614465986));
#9886=CARTESIAN_POINT('Ctrl Pts',(6.63469107356441,1.72995836404769,0.605216415547348));
#9887=CARTESIAN_POINT('Ctrl Pts',(5.36600428635241,1.73653511802878,0.605201749988751));
#9888=CARTESIAN_POINT('Ctrl Pts',(4.10000000006189,1.66887738587128,0.605315322687833));
#9889=CARTESIAN_POINT('Ctrl Pts',(4.08978435969213,1.70060618339657,-0.000163349821525811));
#9890=CARTESIAN_POINT('Ctrl Pts',(4.093189474458,1.69002990998177,0.201662875584159));
#9891=CARTESIAN_POINT('Ctrl Pts',(4.0965946873723,1.67945364446992,0.403489099757173));
#9892=CARTESIAN_POINT('Ctrl Pts',(4.1,1.66887738702936,0.605315322680078));
#9893=CARTESIAN_POINT('Ctrl Pts',(5.36191629113061,1.76821426155324,6.25990704884337E-5));
#9894=CARTESIAN_POINT('Ctrl Pts',(5.3630514496163,1.75763653340724,0.201889184585558));
#9895=CARTESIAN_POINT('Ctrl Pts',(5.36418670607087,1.74705878400967,0.403715765068683));
#9896=CARTESIAN_POINT('Ctrl Pts',(5.36532191986745,1.73648104871457,0.605542351516858));
#9897=CARTESIAN_POINT('Ctrl Pts',(6.63535348785608,1.76179300730897,3.38749616628245E-5));
#9898=CARTESIAN_POINT('Ctrl Pts',(6.63422081650235,1.75121562356675,0.20186041917081));
#9899=CARTESIAN_POINT('Ctrl Pts',(6.63308817234583,1.74063821462875,0.403686959568233));
#9900=CARTESIAN_POINT('Ctrl Pts',(6.63195543348166,1.7300608292057,0.605513504373875));
#9901=CARTESIAN_POINT('Ctrl Pts',(7.91019312949454,1.70715885937616,-0.000134060602928919));
#9902=CARTESIAN_POINT('Ctrl Pts',(7.90679525186394,1.69658223815078,0.201692207018782));
#9903=CARTESIAN_POINT('Ctrl Pts',(7.90339729485302,1.68600562209044,0.403518473580683));
#9904=CARTESIAN_POINT('Ctrl Pts',(7.89999925719352,1.67542901130525,0.605344739067286));
#9905=CARTESIAN_POINT('Origin',(3.9,1.7662962962963,0.));
#9906=CARTESIAN_POINT('',(3.9,-1.657567947596,0.605334330700044));
#9907=CARTESIAN_POINT('Ctrl Pts',(3.9,-1.657567947596,0.605334330700044));
#9908=CARTESIAN_POINT('Ctrl Pts',(3.9,-1.66295505583237,0.504667750148195));
#9909=CARTESIAN_POINT('Ctrl Pts',(3.9,-1.66834175427306,0.404000185805616));
#9910=CARTESIAN_POINT('Ctrl Pts',(3.9,-1.67913790341918,0.202222727053817));
#9911=CARTESIAN_POINT('Ctrl Pts',(3.9,-1.68454745406112,0.101110889248462));
#9912=CARTESIAN_POINT('Ctrl Pts',(3.9,-1.68995649764597,0.));
#9913=CARTESIAN_POINT('',(3.9,-1.55753217754889,0.7));
#9914=CARTESIAN_POINT('Ctrl Pts',(3.89999999700315,-1.55753217437,0.7));
#9915=CARTESIAN_POINT('Ctrl Pts',(3.89999999197785,-1.56545359401377,0.699999998841372));
#9916=CARTESIAN_POINT('Ctrl Pts',(3.90000117861029,-1.57331197233837,0.699006163267487));
#9917=CARTESIAN_POINT('Ctrl Pts',(3.90000221019459,-1.58096665047841,0.697118921400131));
#9918=CARTESIAN_POINT('Ctrl Pts',(3.90000279139136,-1.58527931230009,0.696055645348449));
#9919=CARTESIAN_POINT('Ctrl Pts',(3.90000331912093,-1.58952737074567,0.694707745526415));
#9920=CARTESIAN_POINT('Ctrl Pts',(3.90000364796674,-1.59368396010392,0.693086194530447));
#9921=CARTESIAN_POINT('Ctrl Pts',(3.90000423564848,-1.60111221870485,0.690188313817561));
#9922=CARTESIAN_POINT('Ctrl Pts',(3.90000407815102,-1.60816848972648,0.686450841450731));
#9923=CARTESIAN_POINT('Ctrl Pts',(3.9000032813392,-1.6147063365644,0.681954558458482));
#9924=CARTESIAN_POINT('Ctrl Pts',(3.90000284137901,-1.61831621321653,0.679471932695374));
#9925=CARTESIAN_POINT('Ctrl Pts',(3.90000222202081,-1.62176776859012,0.67675708350434));
#9926=CARTESIAN_POINT('Ctrl Pts',(3.9000016760669,-1.6250323621476,0.673818036286869));
#9927=CARTESIAN_POINT('Ctrl Pts',(3.90000114791654,-1.62819049732732,0.670974831382826));
#9928=CARTESIAN_POINT('Ctrl Pts',(3.90000068451114,-1.63115458712464,0.667938911589952));
#9929=CARTESIAN_POINT('Ctrl Pts',(3.90000068976928,-1.6339023205034,0.664721489040691));
#9930=CARTESIAN_POINT('Ctrl Pts',(3.90000069956116,-1.63901923218135,0.658729908073458));
#9931=CARTESIAN_POINT('Ctrl Pts',(3.9000021571807,-1.64338878348726,0.652110283780478));
#9932=CARTESIAN_POINT('Ctrl Pts',(3.90000267296827,-1.64695081636755,0.645027851744832));
#9933=CARTESIAN_POINT('Ctrl Pts',(3.90000272641596,-1.64731992654249,0.644293945625623));
#9934=CARTESIAN_POINT('Ctrl Pts',(3.90000277224081,-1.64768032438231,0.643555049900053));
#9935=CARTESIAN_POINT('Ctrl Pts',(3.90000280957334,-1.64803191324525,0.642811337026806));
#9936=CARTESIAN_POINT('Ctrl Pts',(3.90000316967295,-1.65142324611312,0.635637680016741));
#9937=CARTESIAN_POINT('Ctrl Pts',(3.90000247513984,-1.65395957542788,0.628100801230905));
#9938=CARTESIAN_POINT('Ctrl Pts',(3.90000142932204,-1.65558732484325,0.62036898832433));
#9939=CARTESIAN_POINT('Ctrl Pts',(3.90000076044003,-1.65662839749185,0.615423891207338));
#9940=CARTESIAN_POINT('Ctrl Pts',(3.9,-1.65729694754734,0.61039839235075));
#9941=CARTESIAN_POINT('Ctrl Pts',(3.9,-1.657567947596,0.605334330700044));
#9942=CARTESIAN_POINT('',(3.9,1.55753217754922,0.7));
#9943=CARTESIAN_POINT('',(3.9,0.883148148148148,0.7));
#9944=CARTESIAN_POINT('',(3.9,1.657567947596,0.605334330700044));
#9945=CARTESIAN_POINT('Ctrl Pts',(3.9,1.657567947596,0.605334330700044));
#9946=CARTESIAN_POINT('Ctrl Pts',(3.9,1.65714453107083,0.613246533660879));
#9947=CARTESIAN_POINT('Ctrl Pts',(3.90000169450566,1.65575314729854,0.621067109624563));
#9948=CARTESIAN_POINT('Ctrl Pts',(3.900002426785,1.653477907766,0.628635640467799));
#9949=CARTESIAN_POINT('Ctrl Pts',(3.90000283370343,1.65221358571927,0.632841378048222));
#9950=CARTESIAN_POINT('Ctrl Pts',(3.90000300372053,1.65067534627202,0.636969322077829));
#9951=CARTESIAN_POINT('Ctrl Pts',(3.90000288278183,1.6488710006323,0.640990000951852));
#9952=CARTESIAN_POINT('Ctrl Pts',(3.90000266510116,1.6456233127241,0.64822692378658));
#9953=CARTESIAN_POINT('Ctrl Pts',(3.90000136145047,1.64155197609259,0.655037842274187));
#9954=CARTESIAN_POINT('Ctrl Pts',(3.9000008487987,1.63672139510901,0.661259788874982));
#9955=CARTESIAN_POINT('Ctrl Pts',(3.90000075195303,1.63580884415802,0.662435184403355));
#9956=CARTESIAN_POINT('Ctrl Pts',(3.90000069125178,1.63486906637168,0.663589490553999));
#9957=CARTESIAN_POINT('Ctrl Pts',(3.90000068992127,1.63390232051248,0.664721489040685));
#9958=CARTESIAN_POINT('Ctrl Pts',(3.90000068733544,1.63202347103487,0.666921503393101));
#9959=CARTESIAN_POINT('Ctrl Pts',(3.9000009071255,1.6300427915863,0.669037305429552));
#9960=CARTESIAN_POINT('Ctrl Pts',(3.90000121037842,1.62796736695056,0.671065303566633));
#9961=CARTESIAN_POINT('Ctrl Pts',(3.90000204102081,1.62228255539437,0.676620208836154));
#9962=CARTESIAN_POINT('Ctrl Pts',(3.90000335328325,1.61595386407616,0.681456575151491));
#9963=CARTESIAN_POINT('Ctrl Pts',(3.90000380482706,1.60914557515952,0.685520902406533));
#9964=CARTESIAN_POINT('Ctrl Pts',(3.90000409284089,1.60480295930069,0.688113302965514));
#9965=CARTESIAN_POINT('Ctrl Pts',(3.90000408819389,1.6002642541482,0.690390927291682));
#9966=CARTESIAN_POINT('Ctrl Pts',(3.90000378365133,1.59556629223371,0.692330537597694));
#9967=CARTESIAN_POINT('Ctrl Pts',(3.90000330864444,1.58823869807682,0.695355823328757));
#9968=CARTESIAN_POINT('Ctrl Pts',(3.90000209726118,1.58060840086481,0.697526456028474));
#9969=CARTESIAN_POINT('Ctrl Pts',(3.90000112250675,1.5728228815436,0.698773197673241));
#9970=CARTESIAN_POINT('Ctrl Pts',(3.90000049100668,1.56777898966077,0.699580906164169));
#9971=CARTESIAN_POINT('Ctrl Pts',(3.89999999374416,1.56266934880282,0.69999999924861));
#9972=CARTESIAN_POINT('Ctrl Pts',(3.89999999700315,1.55753217437,0.7));
#9973=CARTESIAN_POINT('Ctrl Pts',(3.9,1.68995649764597,0.));
#9974=CARTESIAN_POINT('Ctrl Pts',(3.9,1.68454744095908,0.101111134163871));
#9975=CARTESIAN_POINT('Ctrl Pts',(3.9,1.67913787721413,0.202223216861756));
#9976=CARTESIAN_POINT('Ctrl Pts',(3.9,1.66834172806373,0.404000675610066));
#9977=CARTESIAN_POINT('Ctrl Pts',(3.9,1.66295504272671,0.504667995047933));
#9978=CARTESIAN_POINT('Ctrl Pts',(3.9,1.657567947596,0.605334330700044));
#9979=CARTESIAN_POINT('Ctrl Pts',(3.90000000000029,-1.68995649764598,2.25514051876985E-17));
#9980=CARTESIAN_POINT('Ctrl Pts',(3.90375240214247,-1.67935614215062,0.202290156525516));
#9981=CARTESIAN_POINT('Ctrl Pts',(3.90750491350916,-1.66875579641967,0.404580311547879));
#9982=CARTESIAN_POINT('Ctrl Pts',(3.91125753584366,-1.65815546066147,0.606870465045848));
#9983=CARTESIAN_POINT('Ctrl Pts',(2.95719731373254,-1.63434162994996,-0.000186284957671625));
#9984=CARTESIAN_POINT('Ctrl Pts',(2.96263618266967,-1.62374249289717,0.202103577800055));
#9985=CARTESIAN_POINT('Ctrl Pts',(2.96807524459186,-1.6131433886527,0.404393433349269));
#9986=CARTESIAN_POINT('Ctrl Pts',(2.97351444051957,-1.60254429060724,0.606683290324339));
#9987=CARTESIAN_POINT('Ctrl Pts',(2.0151035222252,-1.5373601393942,-0.000515615972119944));
#9988=CARTESIAN_POINT('Ctrl Pts',(2.0222299762717,-1.52676329064944,0.20177372753372));
#9989=CARTESIAN_POINT('Ctrl Pts',(2.02935668076532,-1.51616649670304,0.404063061036967));
#9990=CARTESIAN_POINT('Ctrl Pts',(2.03648357820815,-1.50556972342972,0.606352393906678));
#9991=CARTESIAN_POINT('Ctrl Pts',(1.07355614839761,-1.3885225322474,-0.00102014041634142));
#9992=CARTESIAN_POINT('Ctrl Pts',(1.08237048982668,-1.37792954541675,0.201268457136957));
#9993=CARTESIAN_POINT('Ctrl Pts',(1.09118510562603,-1.36733662501784,0.403557046289628));
#9994=CARTESIAN_POINT('Ctrl Pts',(1.09999999998551,-1.35674377243019,0.605845626932519));
#9995=CARTESIAN_POINT('Ctrl Pts',(1.10000000359112,-1.35674374984279,0.605845627045242));
#9996=CARTESIAN_POINT('Ctrl Pts',(2.02777573897866,-1.50422778688462,0.60559460123127));
#9997=CARTESIAN_POINT('Ctrl Pts',(2.96295221054883,-1.60165319397541,0.605428415101273));
#9998=CARTESIAN_POINT('Ctrl Pts',(3.9,-1.657567947596,0.605334330700044));
#9999=CARTESIAN_POINT('Ctrl Pts',(3.90594750914669,-1.55788759822396,0.7));
#10000=CARTESIAN_POINT('Ctrl Pts',(2.96654482017732,-1.50183737247472,0.7));
#10001=CARTESIAN_POINT('Ctrl Pts',(2.02939151553635,-1.40396309164617,0.7));
#10002=CARTESIAN_POINT('Ctrl Pts',(1.1,-1.25565664448621,0.7));
#10003=CARTESIAN_POINT('Ctrl Pts',(3.90422602671531,-1.58673967158186,0.7));
#10004=CARTESIAN_POINT('Ctrl Pts',(2.9639697519154,-1.53062009474021,0.699999324449154));
#10005=CARTESIAN_POINT('Ctrl Pts',(2.02587169016863,-1.43262076012027,0.700001792708215));
#10006=CARTESIAN_POINT('Ctrl Pts',(1.09546090287069,-1.28410178925883,0.700000000000001));
#10007=CARTESIAN_POINT('Ctrl Pts',(3.90124198563808,-1.6367522482393,0.676652244116846));
#10008=CARTESIAN_POINT('Ctrl Pts',(2.95951584878018,-1.58051528054544,0.676683243227538));
#10009=CARTESIAN_POINT('Ctrl Pts',(2.01975879699698,-1.48229505764113,0.676737195552829));
#10010=CARTESIAN_POINT('Ctrl Pts',(1.08759175402576,-1.33341535796084,0.676819902351873));
#10011=CARTESIAN_POINT('Ctrl Pts',(3.90006887217438,-1.65641364884095,0.626981005337021));
#10012=CARTESIAN_POINT('Ctrl Pts',(2.95775794493813,-1.6001648299169,0.627061170854983));
#10013=CARTESIAN_POINT('Ctrl Pts',(2.01735267249256,-1.50192280897576,0.627202240820629));
#10014=CARTESIAN_POINT('Ctrl Pts',(1.08446813262788,-1.35299014570964,0.627416665943555));
#10015=CARTESIAN_POINT('Ctrl Pts',(3.9,-1.657567947596,0.605334330700044));
#10016=CARTESIAN_POINT('Ctrl Pts',(2.95765589353472,-1.60133715645388,0.605428946878649));
#10017=CARTESIAN_POINT('Ctrl Pts',(2.01720431860088,-1.50312513840151,0.605596482146283));
#10018=CARTESIAN_POINT('Ctrl Pts',(1.0842689834292,-1.35423815332579,0.605849891671036));
#10019=CARTESIAN_POINT('Ctrl Pts',(3.89999999700313,-1.55753217437,0.7));
#10020=CARTESIAN_POINT('Ctrl Pts',(2.96258932077475,-1.50142404037792,0.7));
#10021=CARTESIAN_POINT('Ctrl Pts',(2.02743012901897,-1.40365010593343,0.7));
#10022=CARTESIAN_POINT('Ctrl Pts',(1.1,-1.25565664448621,0.7));
#10023=CARTESIAN_POINT('Origin',(6.08012166120517,1.06778195214465E-16,
0.7));
#10024=CARTESIAN_POINT('Ctrl Pts',(1.1,1.25565664448621,0.7));
#10025=CARTESIAN_POINT('Ctrl Pts',(2.02743012901899,1.40365010593344,0.7));
#10026=CARTESIAN_POINT('Ctrl Pts',(2.96258932077472,1.50142404037792,0.7));
#10027=CARTESIAN_POINT('Ctrl Pts',(3.89999999700315,1.55753217437,0.7));
#10028=CARTESIAN_POINT('Ctrl Pts',(1.1,1.25565664448621,0.7));
#10029=CARTESIAN_POINT('Ctrl Pts',(2.02939151553637,1.40396309164617,0.7));
#10030=CARTESIAN_POINT('Ctrl Pts',(2.96654482017727,1.50183737247472,0.7));
#10031=CARTESIAN_POINT('Ctrl Pts',(3.90594750914669,1.55788759822396,0.7));
#10032=CARTESIAN_POINT('Ctrl Pts',(1.09546090287069,1.28410178925883,0.700000000000001));
#10033=CARTESIAN_POINT('Ctrl Pts',(2.02587169016866,1.43262076012027,0.700001792708215));
#10034=CARTESIAN_POINT('Ctrl Pts',(2.96396975191535,1.53062009474021,0.699999324449154));
#10035=CARTESIAN_POINT('Ctrl Pts',(3.90422602671531,1.58673967158186,0.7));
#10036=CARTESIAN_POINT('Ctrl Pts',(1.08759175402576,1.33341535796084,0.676819902351873));
#10037=CARTESIAN_POINT('Ctrl Pts',(2.019758796997,1.48229505764113,0.676737195552829));
#10038=CARTESIAN_POINT('Ctrl Pts',(2.95951584878014,1.58051528054544,0.676683243227538));
#10039=CARTESIAN_POINT('Ctrl Pts',(3.90124198563808,1.6367522482393,0.676652244116846));
#10040=CARTESIAN_POINT('Ctrl Pts',(1.08446813262788,1.35299014570964,0.627416665943555));
#10041=CARTESIAN_POINT('Ctrl Pts',(2.01735267249258,1.50192280897576,0.627202240820629));
#10042=CARTESIAN_POINT('Ctrl Pts',(2.95775794493809,1.6001648299169,0.627061170854983));
#10043=CARTESIAN_POINT('Ctrl Pts',(3.90006887217438,1.65641364884095,0.626981005337021));
#10044=CARTESIAN_POINT('Ctrl Pts',(1.0842689834292,1.35423815332579,0.605849891671036));
#10045=CARTESIAN_POINT('Ctrl Pts',(2.0172043186009,1.50312513840152,0.605596482146283));
#10046=CARTESIAN_POINT('Ctrl Pts',(2.95765589353468,1.60133715645387,0.605428946878649));
#10047=CARTESIAN_POINT('Ctrl Pts',(3.9,1.657567947596,0.605334330700044));
#10048=CARTESIAN_POINT('Ctrl Pts',(3.9,1.657567947596,0.605334330700044));
#10049=CARTESIAN_POINT('Ctrl Pts',(2.96295221054879,1.60165319397541,0.605428415101273));
#10050=CARTESIAN_POINT('Ctrl Pts',(2.02777573897867,1.50422778688462,0.60559460123127));
#10051=CARTESIAN_POINT('Ctrl Pts',(1.10000000359111,1.35674374984279,0.605845627045242));
#10052=CARTESIAN_POINT('Ctrl Pts',(1.07355614839761,1.3885225322474,-0.00102014041634139));
#10053=CARTESIAN_POINT('Ctrl Pts',(1.08237048982668,1.37792954541676,0.201268457136957));
#10054=CARTESIAN_POINT('Ctrl Pts',(1.09118510562602,1.36733662501784,0.403557046289628));
#10055=CARTESIAN_POINT('Ctrl Pts',(1.09999999998551,1.35674377243019,0.605845626932519));
#10056=CARTESIAN_POINT('Ctrl Pts',(2.0151035222252,1.5373601393942,-0.000515615972119942));
#10057=CARTESIAN_POINT('Ctrl Pts',(2.0222299762717,1.52676329064944,0.201773727533721));
#10058=CARTESIAN_POINT('Ctrl Pts',(2.02935668076532,1.51616649670304,0.404063061036968));
#10059=CARTESIAN_POINT('Ctrl Pts',(2.03648357820815,1.50556972342972,0.606352393906678));
#10060=CARTESIAN_POINT('Ctrl Pts',(2.95719731373254,1.63434162994996,-0.000186284957671606));
#10061=CARTESIAN_POINT('Ctrl Pts',(2.96263618266967,1.62374249289717,0.202103577800055));
#10062=CARTESIAN_POINT('Ctrl Pts',(2.96807524459186,1.6131433886527,0.404393433349269));
#10063=CARTESIAN_POINT('Ctrl Pts',(2.97351444051957,1.60254429060724,0.60668329032434));
#10064=CARTESIAN_POINT('Ctrl Pts',(3.90000000000029,1.68995649764598,4.33680868994202E-17));
#10065=CARTESIAN_POINT('Ctrl Pts',(3.90375240214247,1.67935614215062,0.202290156525516));
#10066=CARTESIAN_POINT('Ctrl Pts',(3.90750491350917,1.66875579641967,0.404580311547879));
#10067=CARTESIAN_POINT('Ctrl Pts',(3.91125753584366,1.65815546066147,0.606870465045848));
#10068=CARTESIAN_POINT('Origin',(0.9,1.44962962962963,0.));
#10069=CARTESIAN_POINT('',(0.900000000000025,-1.32415632515176,0.605901073595307));
#10070=CARTESIAN_POINT('Ctrl Pts',(0.900000000000025,-1.32415632515176,
0.605901073595307));
#10071=CARTESIAN_POINT('Ctrl Pts',(0.900000000000025,-1.33021622058432,
0.504787384877132));
#10072=CARTESIAN_POINT('Ctrl Pts',(0.900000000000001,-1.33627289299046,
0.403672458220672));
#10073=CARTESIAN_POINT('Ctrl Pts',(0.900000000000001,-1.3483639425303,0.201706128802639));
#10074=CARTESIAN_POINT('Ctrl Pts',(0.9,-1.3543984610184,0.100852646477479));
#10075=CARTESIAN_POINT('Ctrl Pts',(0.9,-1.3604297237941,0.));
#10076=CARTESIAN_POINT('',(0.9,-1.22294421121193,0.7));
#10077=CARTESIAN_POINT('Ctrl Pts',(0.899999998934589,-1.2229442093848,0.7));
#10078=CARTESIAN_POINT('Ctrl Pts',(0.89999998269596,-1.2309559991361,0.699999991698178));
#10079=CARTESIAN_POINT('Ctrl Pts',(0.900003161357076,-1.2389110096839,0.699008412490225));
#10080=CARTESIAN_POINT('Ctrl Pts',(0.900005837532895,-1.24666554379878,
0.697120920272419));
#10081=CARTESIAN_POINT('Ctrl Pts',(0.900007138246235,-1.25043451364619,
0.69620353424371));
#10082=CARTESIAN_POINT('Ctrl Pts',(0.900008321383585,-1.25415610217771,
0.695073675615989));
#10083=CARTESIAN_POINT('Ctrl Pts',(0.900009136546862,-1.25781268161099,
0.69373809091454));
#10084=CARTESIAN_POINT('Ctrl Pts',(0.90001081442992,-1.26533916477404,0.690989003700189));
#10085=CARTESIAN_POINT('Ctrl Pts',(0.900010659344479,-1.27251458345821,
0.687399440976464));
#10086=CARTESIAN_POINT('Ctrl Pts',(0.900008585023094,-1.27919110928202,
0.68304500924512));
#10087=CARTESIAN_POINT('Ctrl Pts',(0.900007251085311,-1.28348459539356,
0.680244796581297));
#10088=CARTESIAN_POINT('Ctrl Pts',(0.900005156998288,-1.28757155292352,
0.67712723751572));
#10089=CARTESIAN_POINT('Ctrl Pts',(0.900003422242992,-1.29140570811059,
0.673703384872626));
#10090=CARTESIAN_POINT('Ctrl Pts',(0.90000203719427,-1.29446694202502,0.670969741262059));
#10091=CARTESIAN_POINT('Ctrl Pts',(0.90000088611098,-1.29734878548314,0.668056850549005));
#10092=CARTESIAN_POINT('Ctrl Pts',(0.900000936626746,-1.30003070819003,
0.664973821719563));
#10093=CARTESIAN_POINT('Ctrl Pts',(0.90000103432908,-1.30521780373233,0.659010948495488));
#10094=CARTESIAN_POINT('Ctrl Pts',(0.900005119671874,-1.30966005175478,
0.652412896960716));
#10095=CARTESIAN_POINT('Ctrl Pts',(0.900006662646281,-1.31329014967729,
0.64534035177384));
#10096=CARTESIAN_POINT('Ctrl Pts',(0.900006837929091,-1.31370253096037,
0.644536906434065));
#10097=CARTESIAN_POINT('Ctrl Pts',(0.900006988901759,-1.3141043809937,0.64372731654354));
#10098=CARTESIAN_POINT('Ctrl Pts',(0.900007112770807,-1.31449556093743,
0.642911804846506));
#10099=CARTESIAN_POINT('Ctrl Pts',(0.900008198175579,-1.31792328224658,
0.635765868899185));
#10100=CARTESIAN_POINT('Ctrl Pts',(0.900006415208278,-1.32049402672979,
0.628253543462219));
#10101=CARTESIAN_POINT('Ctrl Pts',(0.900003664797616,-1.32215034643222,
0.620540220943237));
#10102=CARTESIAN_POINT('Ctrl Pts',(0.900001948338234,-1.32318401225236,
0.615726538031782));
#10103=CARTESIAN_POINT('Ctrl Pts',(0.900000000000001,-1.32386068836271,
0.610833984830158));
#10104=CARTESIAN_POINT('Ctrl Pts',(0.900000000000001,-1.32415632515176,
0.605901073595307));
#10105=CARTESIAN_POINT('',(0.9,1.22294421121193,0.7));
#10106=CARTESIAN_POINT('',(0.9,0.724814814814815,0.7));
#10107=CARTESIAN_POINT('',(0.900000000000027,1.32415632515176,0.605901073595307));
#10108=CARTESIAN_POINT('Ctrl Pts',(0.900000000000001,1.32415632515176,0.605901073595307));
#10109=CARTESIAN_POINT('Ctrl Pts',(0.900000000000001,1.32368299187747,0.613798977756921));
#10110=CARTESIAN_POINT('Ctrl Pts',(0.900004523569871,1.32223544152535,0.621596324701597));
#10111=CARTESIAN_POINT('Ctrl Pts',(0.900006356724635,1.31990036466821,0.629134362570908));
#10112=CARTESIAN_POINT('Ctrl Pts',(0.900007328861843,1.3186620540024,0.633131846706937));
#10113=CARTESIAN_POINT('Ctrl Pts',(0.900007702029268,1.31717322147439,0.637056437951431));
#10114=CARTESIAN_POINT('Ctrl Pts',(0.900007358328755,1.31544117393516,0.640882963165587));
#10115=CARTESIAN_POINT('Ctrl Pts',(0.900006707239278,1.31216006761937,0.648131745755711));
#10116=CARTESIAN_POINT('Ctrl Pts',(0.900003091243194,1.3080468004769,0.654946293188228));
#10117=CARTESIAN_POINT('Ctrl Pts',(0.900001489347898,1.30317324258861,0.661167512355852));
#10118=CARTESIAN_POINT('Ctrl Pts',(0.900001155878064,1.30215870403359,0.662462596327245));
#10119=CARTESIAN_POINT('Ctrl Pts',(0.90000093695446,1.30111105636563,0.663731893727214));
#10120=CARTESIAN_POINT('Ctrl Pts',(0.90000091848414,1.30003070515708,0.664973821721807));
#10121=CARTESIAN_POINT('Ctrl Pts',(0.90000089007412,1.29836896897911,0.666884086330845));
#10122=CARTESIAN_POINT('Ctrl Pts',(0.900001333486324,1.29662987445651,0.668729618924651));
#10123=CARTESIAN_POINT('Ctrl Pts',(0.900001997973453,1.2948182721625,0.670508241825176));
#10124=CARTESIAN_POINT('Ctrl Pts',(0.900004083621534,1.28913213515815,0.676090865298813));
#10125=CARTESIAN_POINT('Ctrl Pts',(0.900007925915178,1.28279871831387,0.680954424681199));
#10126=CARTESIAN_POINT('Ctrl Pts',(0.900009431597099,1.27598654051802,0.685053039288488));
#10127=CARTESIAN_POINT('Ctrl Pts',(0.900010426918848,1.2714833923965,0.687762403198649));
#10128=CARTESIAN_POINT('Ctrl Pts',(0.900010579450444,1.26676996242859,0.690136867340003));
#10129=CARTESIAN_POINT('Ctrl Pts',(0.900009885932263,1.26188774903006,0.692153145632694));
#10130=CARTESIAN_POINT('Ctrl Pts',(0.900008832351734,1.25447077696631,0.695216239878874));
#10131=CARTESIAN_POINT('Ctrl Pts',(0.900005746465811,1.24674633448708,0.697421320974322));
#10132=CARTESIAN_POINT('Ctrl Pts',(0.900003140090462,1.23886595492982,0.6987028844583));
#10133=CARTESIAN_POINT('Ctrl Pts',(0.900001403206082,1.23361448254879,0.699556916322089));
#10134=CARTESIAN_POINT('Ctrl Pts',(0.899999988093253,1.22829309040712,0.699999994457486));
#10135=CARTESIAN_POINT('Ctrl Pts',(0.899999998934588,1.2229442093848,0.7));
#10136=CARTESIAN_POINT('Ctrl Pts',(0.9,1.3604297237941,0.));
#10137=CARTESIAN_POINT('Ctrl Pts',(0.9,1.35439838926384,0.100853846331769));
#10138=CARTESIAN_POINT('Ctrl Pts',(0.9,1.34836379894337,0.201708528537181));
#10139=CARTESIAN_POINT('Ctrl Pts',(0.9,1.33627274925098,0.403674857922336));
#10140=CARTESIAN_POINT('Ctrl Pts',(0.900000000000027,1.33021614867672,0.504788584706939));
#10141=CARTESIAN_POINT('Ctrl Pts',(0.900000000000027,1.32415632515176,0.605901073595307));
#10142=CARTESIAN_POINT('Ctrl Pts',(0.900000000000001,-1.3604297237941,-1.73472347597681E-18));
#10143=CARTESIAN_POINT('Ctrl Pts',(0.909119345746934,-1.34984469470005,
0.202150401646216));
#10144=CARTESIAN_POINT('Ctrl Pts',(0.918238975454288,-1.33925973741039,
0.404300794324169));
#10145=CARTESIAN_POINT('Ctrl Pts',(0.92735889343571,-1.32867485341111,0.606451177918334));
#10146=CARTESIAN_POINT('Ctrl Pts',(0.693791632045388,-1.32642527651154,
-0.000115194085079675));
#10147=CARTESIAN_POINT('Ctrl Pts',(0.703280422539661,-1.31584113310577,
0.202035038813999));
#10148=CARTESIAN_POINT('Ctrl Pts',(0.712769508818954,-1.30525706820637,
0.404185262036053));
#10149=CARTESIAN_POINT('Ctrl Pts',(0.722258895242942,-1.29467308328318,
0.606335475483814));
#10150=CARTESIAN_POINT('Ctrl Pts',(0.487608314405001,-1.28990207050556,
-0.000238777108575344));
#10151=CARTESIAN_POINT('Ctrl Pts',(0.497466558273561,-1.27931888757273,
0.201911276725417));
#10152=CARTESIAN_POINT('Ctrl Pts',(0.507325109482935,-1.26873579028159,
0.404061320158324));
#10153=CARTESIAN_POINT('Ctrl Pts',(0.517183972542757,-1.25815278023897,
0.606211353085106));
#10154=CARTESIAN_POINT('Ctrl Pts',(0.281447431601629,-1.2507496025167,-0.000370926150909055));
#10155=CARTESIAN_POINT('Ctrl Pts',(0.291675125201343,-1.24016745708839,
0.201778938960696));
#10156=CARTESIAN_POINT('Ctrl Pts',(0.301903137322998,-1.2295854048496,0.403928792940867));
#10157=CARTESIAN_POINT('Ctrl Pts',(0.312131472716966,-1.21900344770756,
0.606078635650713));
#10158=CARTESIAN_POINT('',(0.313137632044026,-1.21919552599285,0.606079286803921));
#10159=CARTESIAN_POINT('Ctrl Pts',(0.28146619846596,-1.25073018526678,-6.36968776335234E-17));
#10160=CARTESIAN_POINT('Ctrl Pts',(0.292023490345879,-1.2402182973453,0.20202640462578));
#10161=CARTESIAN_POINT('Ctrl Pts',(0.302580635585432,-1.22970674279184,
0.404052833452346));
#10162=CARTESIAN_POINT('Ctrl Pts',(0.313137632044028,-1.21919552599286,
0.606079286803922));
#10163=CARTESIAN_POINT('Ctrl Pts',(0.313137632044026,-1.21919552599285,
0.606079286803921));
#10164=CARTESIAN_POINT('Ctrl Pts',(0.508347756773358,-1.25646926692181,
0.606016122348466));
#10165=CARTESIAN_POINT('Ctrl Pts',(0.703992099548353,-1.29143758865737,
0.605956720831638));
#10166=CARTESIAN_POINT('Ctrl Pts',(0.900000000000031,-1.32415632515176,
0.605901073595307));
#10167=CARTESIAN_POINT('Ctrl Pts',(0.916434425702686,-1.22569269236154,
0.7));
#10168=CARTESIAN_POINT('Ctrl Pts',(0.72117838049967,-1.193102781986,0.7));
#10169=CARTESIAN_POINT('Ctrl Pts',(0.526295996270969,-1.15827411715321,
0.7));
#10170=CARTESIAN_POINT('Ctrl Pts',(0.3318563713692,-1.12115139781564,0.7));
#10171=CARTESIAN_POINT('Ctrl Pts',(0.911693828447622,-1.25409504944868,
0.700000000000001));
#10172=CARTESIAN_POINT('Ctrl Pts',(0.716221724293519,-1.22145811194286,
0.699999606692487));
#10173=CARTESIAN_POINT('Ctrl Pts',(0.52112301919326,-1.18657973614434,0.700000445015345));
#10174=CARTESIAN_POINT('Ctrl Pts',(0.32646265058614,-1.14940237362229,0.699999999999999));
#10175=CARTESIAN_POINT('Ctrl Pts',(0.903473253113197,-1.30334701150065,
0.676847307332805));
#10176=CARTESIAN_POINT('Ctrl Pts',(0.707628846166824,-1.27063023858114,
0.676865462359186));
#10177=CARTESIAN_POINT('Ctrl Pts',(0.512149925983835,-1.23566412474798,
0.676884474751893));
#10178=CARTESIAN_POINT('Ctrl Pts',(0.317109102097966,-1.19839394783867,
0.676905055067496));
#10179=CARTESIAN_POINT('Ctrl Pts',(0.900209809599689,-1.32289929215588,
0.627459885485154));
#10180=CARTESIAN_POINT('Ctrl Pts',(0.704212910592823,-1.29017057588713,
0.627506965865002));
#10181=CARTESIAN_POINT('Ctrl Pts',(0.50858160780484,-1.25519230329596,0.627556915196293));
#10182=CARTESIAN_POINT('Ctrl Pts',(0.31338355686088,-1.21790743260971,0.627610331402299));
#10183=CARTESIAN_POINT('Ctrl Pts',(0.900000000000031,-1.32415632515176,
0.605901073595307));
#10184=CARTESIAN_POINT('Ctrl Pts',(0.703992099548353,-1.29143758865737,
0.605956720831638));
#10185=CARTESIAN_POINT('Ctrl Pts',(0.508347756773358,-1.25646926692181,
0.606016122348466));
#10186=CARTESIAN_POINT('Ctrl Pts',(0.313137632044026,-1.21919552599285,
0.606079286803921));
#10187=CARTESIAN_POINT('',(0.3318563713692,-1.12115139781563,0.7));
#10188=CARTESIAN_POINT('Origin',(0.331856371369202,-1.12115139781563,0.6));
#10189=CARTESIAN_POINT('Ctrl Pts',(0.899999998934586,-1.2229442093848,0.7));
#10190=CARTESIAN_POINT('Ctrl Pts',(0.71024282334811,-1.19114655107378,0.7));
#10191=CARTESIAN_POINT('Ctrl Pts',(0.520840466228891,-1.15723253876768,
0.7));
#10192=CARTESIAN_POINT('Ctrl Pts',(0.3318563713692,-1.12115139781564,0.7));
#10193=CARTESIAN_POINT('Origin',(6.08012166120517,1.06778195214465E-16,
0.7));
#10194=CARTESIAN_POINT('',(0.331856371369203,1.12115139781563,0.7));
#10195=CARTESIAN_POINT('',(0.3318563713692,-0.7,0.7));
#10196=CARTESIAN_POINT('Ctrl Pts',(0.331856371369202,1.12115139781564,0.7));
#10197=CARTESIAN_POINT('Ctrl Pts',(0.520840466228894,1.15723253876768,0.7));
#10198=CARTESIAN_POINT('Ctrl Pts',(0.710242823348114,1.19114655107378,0.7));
#10199=CARTESIAN_POINT('Ctrl Pts',(0.899999998934589,1.2229442093848,0.7));
#10200=CARTESIAN_POINT('Ctrl Pts',(0.281447431601628,1.2507496025167,-0.000370926150909064));
#10201=CARTESIAN_POINT('Ctrl Pts',(0.291675125201342,1.24016745708839,0.201778938960695));
#10202=CARTESIAN_POINT('Ctrl Pts',(0.301903137322998,1.2295854048496,0.403928792940867));
#10203=CARTESIAN_POINT('Ctrl Pts',(0.312131472716965,1.21900344770756,0.606078635650713));
#10204=CARTESIAN_POINT('Ctrl Pts',(0.487608314405001,1.28990207050556,-0.000238777108575355));
#10205=CARTESIAN_POINT('Ctrl Pts',(0.497466558273561,1.27931888757273,0.201911276725417));
#10206=CARTESIAN_POINT('Ctrl Pts',(0.507325109482935,1.26873579028159,0.404061320158324));
#10207=CARTESIAN_POINT('Ctrl Pts',(0.517183972542757,1.25815278023897,0.606211353085106));
#10208=CARTESIAN_POINT('Ctrl Pts',(0.693791632045388,1.32642527651154,-0.000115194085079627));
#10209=CARTESIAN_POINT('Ctrl Pts',(0.703280422539661,1.31584113310577,0.202035038813999));
#10210=CARTESIAN_POINT('Ctrl Pts',(0.712769508818955,1.30525706820637,0.404185262036054));
#10211=CARTESIAN_POINT('Ctrl Pts',(0.722258895242942,1.29467308328318,0.606335475483814));
#10212=CARTESIAN_POINT('Ctrl Pts',(0.900000000000002,1.3604297237941,4.33680868994202E-17));
#10213=CARTESIAN_POINT('Ctrl Pts',(0.909119345746935,1.34984469470005,0.202150401646216));
#10214=CARTESIAN_POINT('Ctrl Pts',(0.918238975454289,1.33925973741039,0.40430079432417));
#10215=CARTESIAN_POINT('Ctrl Pts',(0.927358893435711,1.32867485341111,0.606451177918334));
#10216=CARTESIAN_POINT('',(0.313137632044028,1.21919552599286,0.606079286803921));
#10217=CARTESIAN_POINT('Ctrl Pts',(0.900000000000026,1.32415632515176,0.605901073595307));
#10218=CARTESIAN_POINT('Ctrl Pts',(0.703992099548352,1.29143758865737,0.605956720831638));
#10219=CARTESIAN_POINT('Ctrl Pts',(0.508347756773358,1.25646926692181,0.606016122348466));
#10220=CARTESIAN_POINT('Ctrl Pts',(0.313137632044028,1.21919552599286,0.606079286803921));
#10221=CARTESIAN_POINT('Ctrl Pts',(0.313137632044028,1.21919552599286,0.606079286803922));
#10222=CARTESIAN_POINT('Ctrl Pts',(0.302580635585432,1.22970674279184,0.404052833452346));
#10223=CARTESIAN_POINT('Ctrl Pts',(0.29202349034588,1.2402182973453,0.20202640462578));
#10224=CARTESIAN_POINT('Ctrl Pts',(0.28146619846596,1.25073018526678,-6.5594231435373E-18));
#10225=CARTESIAN_POINT('Ctrl Pts',(0.331856371369202,1.12115139781564,0.7));
#10226=CARTESIAN_POINT('Ctrl Pts',(0.526295996270969,1.15827411715321,0.7));
#10227=CARTESIAN_POINT('Ctrl Pts',(0.72117838049967,1.193102781986,0.7));
#10228=CARTESIAN_POINT('Ctrl Pts',(0.916434425702682,1.22569269236154,0.7));
#10229=CARTESIAN_POINT('Ctrl Pts',(0.326462650586141,1.14940237362229,0.699999999999999));
#10230=CARTESIAN_POINT('Ctrl Pts',(0.52112301919326,1.18657973614434,0.700000445015345));
#10231=CARTESIAN_POINT('Ctrl Pts',(0.716221724293519,1.22145811194286,0.699999606692487));
#10232=CARTESIAN_POINT('Ctrl Pts',(0.911693828447618,1.25409504944868,0.700000000000001));
#10233=CARTESIAN_POINT('Ctrl Pts',(0.317109102097967,1.19839394783867,0.676905055067496));
#10234=CARTESIAN_POINT('Ctrl Pts',(0.512149925983836,1.23566412474798,0.676884474751893));
#10235=CARTESIAN_POINT('Ctrl Pts',(0.707628846166824,1.27063023858114,0.676865462359185));
#10236=CARTESIAN_POINT('Ctrl Pts',(0.903473253113193,1.30334701150065,0.676847307332805));
#10237=CARTESIAN_POINT('Ctrl Pts',(0.313383556860882,1.21790743260971,0.627610331402299));
#10238=CARTESIAN_POINT('Ctrl Pts',(0.508581607804839,1.25519230329596,0.627556915196293));
#10239=CARTESIAN_POINT('Ctrl Pts',(0.704212910592822,1.29017057588713,0.627506965865002));
#10240=CARTESIAN_POINT('Ctrl Pts',(0.900209809599685,1.32289929215587,0.627459885485154));
#10241=CARTESIAN_POINT('Ctrl Pts',(0.313137632044028,1.21919552599286,0.606079286803921));
#10242=CARTESIAN_POINT('Ctrl Pts',(0.508347756773358,1.25646926692181,0.606016122348466));
#10243=CARTESIAN_POINT('Ctrl Pts',(0.703992099548352,1.29143758865737,0.605956720831638));
#10244=CARTESIAN_POINT('Ctrl Pts',(0.900000000000026,1.32415632515176,0.605901073595307));
#10245=CARTESIAN_POINT('Origin',(0.3318563713692,1.12115139781563,0.6));
#10246=CARTESIAN_POINT('Origin',(0.3318563713692,1.12115139781563,0.6));
#10247=CARTESIAN_POINT('Origin',(0.3318563713692,1.12115139781563,0.6));
#10248=CARTESIAN_POINT('Origin',(0.331856371369201,1.12115139781563,0.6));
#10249=CARTESIAN_POINT('Origin',(11.6681436286308,1.2964346619681,0.6));
#10250=CARTESIAN_POINT('Origin',(11.6681436286308,1.2964346619681,0.6));
#10251=CARTESIAN_POINT('',(11.7680065821063,1.2964346619681,0.605233595624295));
#10252=CARTESIAN_POINT('Origin',(11.6681436286308,1.2964346619681,0.6));
#10253=CARTESIAN_POINT('Origin',(11.6681436286308,1.2964346619681,0.6));
#10254=CARTESIAN_POINT('Origin',(0.3318563713692,-1.12115139781563,0.6));
#10255=CARTESIAN_POINT('Origin',(0.3318563713692,-1.12115139781563,0.6));
#10256=CARTESIAN_POINT('Origin',(0.3318563713692,-1.12115139781563,0.6));
#10257=CARTESIAN_POINT('Origin',(0.3318563713692,-0.7,0.6));
#10258=CARTESIAN_POINT('Ctrl Pts',(0.281398851089427,-1.25079724300364,
-0.00128877254616805));
#10259=CARTESIAN_POINT('Ctrl Pts',(0.291978592719145,-1.24026300108396,
0.201167222825305));
#10260=CARTESIAN_POINT('Ctrl Pts',(0.302558187088771,-1.2297290939422,0.403623242499903));
#10261=CARTESIAN_POINT('Ctrl Pts',(0.313137632044028,-1.21919552599286,
0.606079286803922));
#10262=CARTESIAN_POINT('Ctrl Pts',(0.258825925396095,-1.24645021448495,
-0.000331836826913007));
#10263=CARTESIAN_POINT('Ctrl Pts',(0.269412087408768,-1.23590982471973,
0.202123507634926));
#10264=CARTESIAN_POINT('Ctrl Pts',(0.279998097240749,-1.22537010804418,
0.404578894752494));
#10265=CARTESIAN_POINT('Ctrl Pts',(0.290584031570127,-1.21483034200885,
0.60703428203898));
#10266=CARTESIAN_POINT('Ctrl Pts',(0.216858515231733,-1.22156435206688,
0.000573427186746937));
#10267=CARTESIAN_POINT('Ctrl Pts',(0.22746089442761,-1.21102065820065,0.20302778119957));
#10268=CARTESIAN_POINT('Ctrl Pts',(0.238063405890532,-1.20047706879609,
0.405482132943502));
#10269=CARTESIAN_POINT('Ctrl Pts',(0.248665715176951,-1.18993398276804,
0.607936521147589));
#10270=CARTESIAN_POINT('Ctrl Pts',(0.20022524016831,-1.1757120364715,-0.000939345874739115));
#10271=CARTESIAN_POINT('Ctrl Pts',(0.210835545796271,-1.16517845930889,
0.201515175954065));
#10272=CARTESIAN_POINT('Ctrl Pts',(0.221445511453644,-1.15464532122135,
0.403969738345816));
#10273=CARTESIAN_POINT('Ctrl Pts',(0.232055819885544,-1.1441124535127,0.606424296559432));
#10274=CARTESIAN_POINT('Ctrl Pts',(0.200162791320387,-1.15273540576203,
-0.00213094087794781));
#10275=CARTESIAN_POINT('Ctrl Pts',(0.210772999146098,-1.14220702337553,
0.200323884929633));
#10276=CARTESIAN_POINT('Ctrl Pts',(0.221383207999129,-1.13167901896849,
0.402778730339676));
#10277=CARTESIAN_POINT('Ctrl Pts',(0.231993417893744,-1.12115139781563,
0.605233595624295));
#10278=CARTESIAN_POINT('Origin',(11.6681436286308,-1.2964346619681,0.6));
#10279=CARTESIAN_POINT('',(11.7680065821063,-1.2964346619681,0.605233595624295));
#10280=CARTESIAN_POINT('Origin',(11.6681436286308,-1.2964346619681,0.6));
#10281=CARTESIAN_POINT('Origin',(11.6681436286308,-1.2964346619681,0.6));
#10282=CARTESIAN_POINT('Origin',(11.6681436286308,0.8,0.6));
#10283=CARTESIAN_POINT('',(11.7680065821063,0.8,0.605233595624295));
#10284=CARTESIAN_POINT('Ctrl Pts',(11.7998406965532,-1.32812796269332,-0.00219749346969486));
#10285=CARTESIAN_POINT('Ctrl Pts',(11.7892293257052,-1.31756329650235,0.200279524124498));
#10286=CARTESIAN_POINT('Ctrl Pts',(11.778617954226,-1.30699886176745,0.402756553762325));
#10287=CARTESIAN_POINT('Ctrl Pts',(11.7680065821063,-1.2964346619681,0.605233595624295));
#10288=CARTESIAN_POINT('Ctrl Pts',(11.7997644051931,-1.35610429277321,-0.000741767599518841));
#10289=CARTESIAN_POINT('Ctrl Pts',(11.7891529352516,-1.34553639595159,0.201735054786578));
#10290=CARTESIAN_POINT('Ctrl Pts',(11.7785417923834,-1.33496887357233,0.404211913913734));
#10291=CARTESIAN_POINT('Ctrl Pts',(11.7679303202531,-1.32440140973518,0.606688758469115));
#10292=CARTESIAN_POINT('Ctrl Pts',(11.777798894316,-1.40464673224301,0.000639873095493681));
#10293=CARTESIAN_POINT('Ctrl Pts',(11.7671928076068,-1.39407357725403,0.203116666245104));
#10294=CARTESIAN_POINT('Ctrl Pts',(11.7565866683578,-1.38350056680667,0.405593463707878));
#10295=CARTESIAN_POINT('Ctrl Pts',(11.7459806329718,-1.37292778989405,0.608070278434593));
#10296=CARTESIAN_POINT('Ctrl Pts',(11.7305637688674,-1.42539741767755,-0.000752904078362463));
#10297=CARTESIAN_POINT('Ctrl Pts',(11.7199663219939,-1.4148278080644,0.201724510929383));
#10298=CARTESIAN_POINT('Ctrl Pts',(11.7093688723049,-1.40425849106451,0.404201940657439));
#10299=CARTESIAN_POINT('Ctrl Pts',(11.6987715660822,-1.39368929079062,0.606679383299034));
#10300=CARTESIAN_POINT('Ctrl Pts',(11.7096810564041,-1.4274931182575,-0.0017379730583696));
#10301=CARTESIAN_POINT('Ctrl Pts',(11.6990862989954,-1.41692678914967,0.200739752511227));
#10302=CARTESIAN_POINT('Ctrl Pts',(11.6884916259906,-1.40636067879325,0.403217493356832));
#10303=CARTESIAN_POINT('Ctrl Pts',(11.6778970386953,-1.39579479040469,0.605695249702977));
#10304=CARTESIAN_POINT('Ctrl Pts',(11.7997255308004,-1.32801330383774,1.58293517182884E-17));
#10305=CARTESIAN_POINT('Ctrl Pts',(11.7891525485321,-1.31748685893698,0.201744519857947));
#10306=CARTESIAN_POINT('Ctrl Pts',(11.7785795656372,-1.30696064383315,0.403489051673192));
#10307=CARTESIAN_POINT('Ctrl Pts',(11.7680065821063,-1.2964346619681,0.605233595624295));
#10308=CARTESIAN_POINT('Ctrl Pts',(11.7096782931395,1.42749036240749,-0.00168516396645821));
#10309=CARTESIAN_POINT('Ctrl Pts',(11.6990844568337,1.41692495195436,0.200774958575157));
#10310=CARTESIAN_POINT('Ctrl Pts',(11.6884907049172,1.40635976021489,0.403235096390144));
#10311=CARTESIAN_POINT('Ctrl Pts',(11.6778970386953,1.39579479040469,0.605695249702978));
#10312=CARTESIAN_POINT('Ctrl Pts',(11.7375219088137,1.42469609383707,-0.000371738767665111));
#10313=CARTESIAN_POINT('Ctrl Pts',(11.7269244310859,1.41412622652679,0.202087962343291));
#10314=CARTESIAN_POINT('Ctrl Pts',(11.7163270893473,1.40355692684423,0.404547700208143));
#10315=CARTESIAN_POINT('Ctrl Pts',(11.7057297418778,1.39298745758592,0.607007427831054));
#10316=CARTESIAN_POINT('Ctrl Pts',(11.7837126264455,1.39812338730171,0.000662527065309348));
#10317=CARTESIAN_POINT('Ctrl Pts',(11.7731059659782,1.38755170250994,0.203121672627585));
#10318=CARTESIAN_POINT('Ctrl Pts',(11.762499302106,1.37698011891703,0.405580822779681));
#10319=CARTESIAN_POINT('Ctrl Pts',(11.7518926781287,1.36640881816393,0.608039989525598));
#10320=CARTESIAN_POINT('Ctrl Pts',(11.7997807104374,1.34910745421534,-0.00105289019631603));
#10321=CARTESIAN_POINT('Ctrl Pts',(11.7891702365097,1.33854134055748,0.201406383632416));
#10322=CARTESIAN_POINT('Ctrl Pts',(11.7785598611315,1.32797539467558,0.403865671186622));
#10323=CARTESIAN_POINT('Ctrl Pts',(11.7679493857164,1.31740972279341,0.60632496775791));
#10324=CARTESIAN_POINT('Ctrl Pts',(11.7998379289556,1.32812520727701,-0.00214468456243374));
#10325=CARTESIAN_POINT('Ctrl Pts',(11.78922748064,1.31756145959839,0.200314730064766));
#10326=CARTESIAN_POINT('Ctrl Pts',(11.7786170316934,1.30699794333589,0.402774156733522));
#10327=CARTESIAN_POINT('Ctrl Pts',(11.7680065821063,1.2964346619681,0.605233595624295));
#10328=CARTESIAN_POINT('Ctrl Pts',(11.7680065821063,1.2964346619681,0.605233595624295));
#10329=CARTESIAN_POINT('Ctrl Pts',(11.7785795656372,1.30696064383315,0.403489051673192));
#10330=CARTESIAN_POINT('Ctrl Pts',(11.7891525485321,1.31748685893698,0.201744519857946));
#10331=CARTESIAN_POINT('Ctrl Pts',(11.7997255308004,1.32801330383774,3.10081821330854E-17));
#10332=CARTESIAN_POINT('Ctrl Pts',(11.3905090053564,1.32332268868375,0.7));
#10333=CARTESIAN_POINT('Ctrl Pts',(11.4830653488871,1.31448403714216,0.7));
#10334=CARTESIAN_POINT('Ctrl Pts',(11.5756099286391,1.3055179747114,0.7));
#10335=CARTESIAN_POINT('Ctrl Pts',(11.6681436286308,1.2964346619681,0.7));
#10336=CARTESIAN_POINT('Ctrl Pts',(11.3932507170007,1.35203326785047,0.7));
#10337=CARTESIAN_POINT('Ctrl Pts',(11.4858332859074,1.34318985044544,0.699999917777441));
#10338=CARTESIAN_POINT('Ctrl Pts',(11.5784027531871,1.33421922733773,0.700000082825348));
#10339=CARTESIAN_POINT('Ctrl Pts',(11.6709605510772,1.32513126902304,0.7));
#10340=CARTESIAN_POINT('Ctrl Pts',(11.3980029235658,1.40179729139028,0.67675176769038));
#10341=CARTESIAN_POINT('Ctrl Pts',(11.4906306781252,1.39294591144353,0.676755553516685));
#10342=CARTESIAN_POINT('Ctrl Pts',(11.583243842395,1.38396722707511,0.676759299309383));
#10343=CARTESIAN_POINT('Ctrl Pts',(11.6758431636759,1.37487151491717,0.676763114282959));
#10344=CARTESIAN_POINT('Ctrl Pts',(11.3998836071583,1.4214913811319,0.627256563056779));
#10345=CARTESIAN_POINT('Ctrl Pts',(11.4925297866457,1.41264104586547,0.627266369072496));
#10346=CARTESIAN_POINT('Ctrl Pts',(11.5851604051362,1.40366358810601,0.627276165220861));
#10347=CARTESIAN_POINT('Ctrl Pts',(11.6777767156198,1.39456903283364,0.627286048421068));
#10348=CARTESIAN_POINT('Ctrl Pts',(11.4,1.4227102204299,0.605660349289938));
#10349=CARTESIAN_POINT('Ctrl Pts',(11.4926474653491,1.41386220753305,0.605671932550561));
#10350=CARTESIAN_POINT('Ctrl Pts',(11.585279512325,1.40488700096013,0.605683574233495));
#10351=CARTESIAN_POINT('Ctrl Pts',(11.6778970386953,1.39579479040469,0.605695249702977));
#10352=CARTESIAN_POINT('Ctrl Pts',(0.200160078391861,1.15273809776858,-0.00218270663797729));
#10353=CARTESIAN_POINT('Ctrl Pts',(0.210771190526905,1.14220881798213,0.200289374419605));
#10354=CARTESIAN_POINT('Ctrl Pts',(0.221382303689445,1.13167991623912,0.402761475082968));
#10355=CARTESIAN_POINT('Ctrl Pts',(0.231993417893744,1.12115139781563,0.605233595624295));
#10356=CARTESIAN_POINT('Ctrl Pts',(0.200222527243758,1.17571472979894,-0.000991111558954063));
#10357=CARTESIAN_POINT('Ctrl Pts',(0.210833737189325,1.165180254798,0.201480665494204));
#10358=CARTESIAN_POINT('Ctrl Pts',(0.22144460713556,1.15464621893915,0.403952483115279));
#10359=CARTESIAN_POINT('Ctrl Pts',(0.232055819885544,1.1441124535127,0.606424296559433));
#10360=CARTESIAN_POINT('Ctrl Pts',(0.216855804290742,1.22156704800519,0.000521661548984882));
#10361=CARTESIAN_POINT('Ctrl Pts',(0.22745908713481,1.21102245544698,0.202993270772045));
#10362=CARTESIAN_POINT('Ctrl Pts',(0.238062502254218,1.2004779673848,0.405464877727456));
#10363=CARTESIAN_POINT('Ctrl Pts',(0.248665715176951,1.18993398276804,0.607936521147589));
#10364=CARTESIAN_POINT('Ctrl Pts',(0.258823218619159,1.24645290953083,-0.000383602721372307));
#10365=CARTESIAN_POINT('Ctrl Pts',(0.269410282911183,1.23591162135389,0.202088997034388));
#10366=CARTESIAN_POINT('Ctrl Pts',(0.279997195000074,1.22537100634993,0.404561639451295));
#10367=CARTESIAN_POINT('Ctrl Pts',(0.290584031570127,1.21483034200885,0.60703428203898));
#10368=CARTESIAN_POINT('Ctrl Pts',(0.281396145950812,1.25079993650842,-0.00134053860524368));
#10369=CARTESIAN_POINT('Ctrl Pts',(0.291976789318506,1.24026479669674,0.201132712115111));
#10370=CARTESIAN_POINT('Ctrl Pts',(0.302557285401186,1.22972999171968,0.403605987142707));
#10371=CARTESIAN_POINT('Ctrl Pts',(0.313137632044028,1.21919552599286,0.606079286803922));
#10372=CARTESIAN_POINT('Origin',(11.8002740930491,1.6,-0.0104671912485888));
#10373=CARTESIAN_POINT('Origin',(0.3318563713692,1.12115139781563,0.6));
#10374=CARTESIAN_POINT('',(0.331856371369203,1.12115139781563,0.9));
#10375=CARTESIAN_POINT('',(0.0322675109428288,1.12115139781563,0.615700786872883));
#10376=CARTESIAN_POINT('Origin',(0.3318563713692,1.12115139781563,0.6));
#10377=CARTESIAN_POINT('',(0.275700153393682,1.4152837823473,0.618237860411764));
#10378=CARTESIAN_POINT('Origin',(0.3318563713692,1.12115139781563,0.6));
#10379=CARTESIAN_POINT('Origin',(0.331856371369201,1.12115139781563,0.600000000000001));
#10380=CARTESIAN_POINT('Origin',(11.6681436286308,1.2964346619681,0.6));
#10381=CARTESIAN_POINT('',(11.6681436286308,1.2964346619681,0.9));
#10382=CARTESIAN_POINT('',(11.6974038588243,1.59451504727786,0.617085749108931));
#10383=CARTESIAN_POINT('Origin',(11.6681436286308,1.2964346619681,0.6));
#10384=CARTESIAN_POINT('',(11.9677324890572,1.2964346619681,0.615700786872884));
#10385=CARTESIAN_POINT('Origin',(11.6681436286308,1.2964346619681,0.6));
#10386=CARTESIAN_POINT('Origin',(11.6681436286308,1.2964346619681,0.6));
#10387=CARTESIAN_POINT('Origin',(0.3318563713692,-1.12115139781563,0.6));
#10388=CARTESIAN_POINT('',(0.3318563713692,-1.12115139781563,0.9));
#10389=CARTESIAN_POINT('',(0.27570015339368,-1.4152837823473,0.618237860411764));
#10390=CARTESIAN_POINT('Origin',(0.331856371369206,-1.12115139781563,0.6));
#10391=CARTESIAN_POINT('',(0.0322675109428289,-1.12115139781563,0.615700786872884));
#10392=CARTESIAN_POINT('Origin',(0.3318563713692,-1.12115139781563,0.6));
#10393=CARTESIAN_POINT('Origin',(0.331856371369201,-1.12115139781563,0.6));
#10394=CARTESIAN_POINT('Origin',(0.3318563713692,-0.7,0.6));
#10395=CARTESIAN_POINT('',(0.0322675109428288,-0.7,0.615700786872883));
#10396=CARTESIAN_POINT('',(0.3318563713692,-0.7,0.9));
#10397=CARTESIAN_POINT('Ctrl Pts',(0.243379792658812,-1.44768816351885,
-0.00386660544379547));
#10398=CARTESIAN_POINT('Ctrl Pts',(0.254153714020244,-1.43688644166428,
0.203501514337738));
#10399=CARTESIAN_POINT('Ctrl Pts',(0.264927169923045,-1.42608498030896,
0.410869669467268));
#10400=CARTESIAN_POINT('Ctrl Pts',(0.275700153393682,-1.4152837823473,0.618237860411764));
#10401=CARTESIAN_POINT('Ctrl Pts',(0.165985306518657,-1.43278556900406,
-0.000585522405354874));
#10402=CARTESIAN_POINT('Ctrl Pts',(0.176781886982148,-1.42196211044871,
0.206780297826791));
#10403=CARTESIAN_POINT('Ctrl Pts',(0.187577631459021,-1.41114055376332,
0.414146260476818));
#10404=CARTESIAN_POINT('Ctrl Pts',(0.198373523197449,-1.40031743725927,
0.621512129789107));
#10405=CARTESIAN_POINT('Ctrl Pts',(0.0420337764471552,-1.35067831466576,
0.00164062070145552));
#10406=CARTESIAN_POINT('Ctrl Pts',(0.0528811856485653,-1.33984924001505,
0.209003590924217));
#10407=CARTESIAN_POINT('Ctrl Pts',(0.0637288270387668,-1.3290196870647,
0.416366521726085));
#10408=CARTESIAN_POINT('Ctrl Pts',(0.0745760486629849,-1.31819094697801,
0.623729515932473));
#10409=CARTESIAN_POINT('Ctrl Pts',(-0.000174449685670057,-1.21258510413485,
-0.00332869829739982));
#10410=CARTESIAN_POINT('Ctrl Pts',(0.0106931634330696,-1.20178787588112,
0.204035045544629));
#10411=CARTESIAN_POINT('Ctrl Pts',(0.0215603573327632,-1.19099068058357,
0.411398812224037));
#10412=CARTESIAN_POINT('Ctrl Pts',(0.0324279732074593,-1.18019411246525,
0.618762589277523));
#10413=CARTESIAN_POINT('Ctrl Pts',(-0.000335035344191381,-1.15350137313465,
-0.00639285519773308));
#10414=CARTESIAN_POINT('Ctrl Pts',(0.0105324790023165,-1.1427176497384,
0.200971671503832));
#10415=CARTESIAN_POINT('Ctrl Pts',(0.0213999944262164,-1.13193432274319,
0.408336218763261));
#10416=CARTESIAN_POINT('Ctrl Pts',(0.0322675109428286,-1.12115139781563,
0.615700786872884));
#10417=CARTESIAN_POINT('Ctrl Pts',(0.243580684154575,-1.44748675362873,
-2.16840434497101E-17));
#10418=CARTESIAN_POINT('Ctrl Pts',(0.254287635915809,-1.43675217163244,
0.206079251738322));
#10419=CARTESIAN_POINT('Ctrl Pts',(0.264994127943615,-1.42601784692504,
0.412158538389471));
#10420=CARTESIAN_POINT('Ctrl Pts',(0.275700153393682,-1.4152837823473,0.618237860411764));
#10421=CARTESIAN_POINT('Ctrl Pts',(0.0322675109428286,-1.12115139781563,
0.615700786872884));
#10422=CARTESIAN_POINT('Ctrl Pts',(0.0215116728964671,-1.13182351356624,
0.410467170919192));
#10423=CARTESIAN_POINT('Ctrl Pts',(0.0107558359204751,-1.14249602316337,
0.205233575389367));
#10424=CARTESIAN_POINT('Ctrl Pts',(-1.41190227911925E-16,-1.15316892111333,
8.06646416329215E-17));
#10425=CARTESIAN_POINT('Origin',(11.6681436286308,-1.2964346619681,0.6));
#10426=CARTESIAN_POINT('',(11.9677324890572,-1.2964346619681,0.615700786872884));
#10427=CARTESIAN_POINT('',(11.6974038588243,-1.59451504727786,0.617085749108931));
#10428=CARTESIAN_POINT('Origin',(11.6681436286308,-1.2964346619681,0.600000000000001));
#10429=CARTESIAN_POINT('',(11.6681436286308,-1.2964346619681,0.9));
#10430=CARTESIAN_POINT('Origin',(11.6681436286308,-1.2964346619681,0.6));
#10431=CARTESIAN_POINT('Origin',(11.6681436286308,-1.2964346619681,0.6));
#10432=CARTESIAN_POINT('Origin',(11.6681436286308,0.8,0.6));
#10433=CARTESIAN_POINT('',(11.9677324890572,0.8,0.615700786872884));
#10434=CARTESIAN_POINT('',(11.6681436286308,0.8,0.9));
#10435=CARTESIAN_POINT('Ctrl Pts',(11.6681436286308,-1.2964346619681,0.9));
#10436=CARTESIAN_POINT('Ctrl Pts',(10.0505146497799,-1.45522470190849,0.9));
#10437=CARTESIAN_POINT('Ctrl Pts',(7.34698379851713,-1.66064017564263,0.9));
#10438=CARTESIAN_POINT('Ctrl Pts',(3.5507249968367,-1.5921338472202,0.9));
#10439=CARTESIAN_POINT('Ctrl Pts',(1.39628032950236,-1.32437289587156,0.9));
#10440=CARTESIAN_POINT('Ctrl Pts',(0.331856371369199,-1.12115139781563,
0.9));
#10441=CARTESIAN_POINT('Ctrl Pts',(11.6765943959699,-1.38252448313292,0.9));
#10442=CARTESIAN_POINT('Ctrl Pts',(10.0577014803155,-1.54155822929668,0.900004386952174));
#10443=CARTESIAN_POINT('Ctrl Pts',(7.35045927226653,-1.74750661992774,0.90000020513805));
#10444=CARTESIAN_POINT('Ctrl Pts',(3.54497585078588,-1.67885197560093,0.899998846478116));
#10445=CARTESIAN_POINT('Ctrl Pts',(1.38372480803625,-1.41002339692611,0.900007381454799));
#10446=CARTESIAN_POINT('Ctrl Pts',(0.315675209020016,-1.2059043252356,0.9));
#10447=CARTESIAN_POINT('Ctrl Pts',(11.6912432102654,-1.53175516862908,0.830242007927396));
#10448=CARTESIAN_POINT('Ctrl Pts',(10.070172518288,-1.69119563674726,0.830042231904815));
#10449=CARTESIAN_POINT('Ctrl Pts',(7.35645297288469,-1.89806162871739,0.829725685238203));
#10450=CARTESIAN_POINT('Ctrl Pts',(3.53503777381493,-1.8291593714544,0.829829026055289));
#10451=CARTESIAN_POINT('Ctrl Pts',(1.36192166831068,-1.55847530615989,0.830279056498203));
#10452=CARTESIAN_POINT('Ctrl Pts',(0.28762358730286,-1.35283178372728,0.830616544072481));
#10453=CARTESIAN_POINT('Ctrl Pts',(11.6970428895979,-1.59083777456472,0.681858145263203));
#10454=CARTESIAN_POINT('Ctrl Pts',(10.0750816081461,-1.75021732245097,0.681339641080976));
#10455=CARTESIAN_POINT('Ctrl Pts',(7.3588078744758,-1.95708146899443,0.680519979048775));
#10456=CARTESIAN_POINT('Ctrl Pts',(3.53113644431293,-1.88819699008302,0.68078748362792));
#10457=CARTESIAN_POINT('Ctrl Pts',(1.35331700817769,-1.61730376958615,0.681953432622034));
#10458=CARTESIAN_POINT('Ctrl Pts',(0.276437927844241,-1.41141950219787,
0.682830994206899));
#10459=CARTESIAN_POINT('Ctrl Pts',(11.6974038588243,-1.59451504727786,0.617085749108931));
#10460=CARTESIAN_POINT('Ctrl Pts',(10.0753786444688,-1.75377172884558,0.616473434532366));
#10461=CARTESIAN_POINT('Ctrl Pts',(7.35893161235257,-1.96044797105896,0.61550283428964));
#10462=CARTESIAN_POINT('Ctrl Pts',(3.53092277948893,-1.89162724517065,0.615818637525046));
#10463=CARTESIAN_POINT('Ctrl Pts',(1.35277799022997,-1.62098550016515,0.617200513836093));
#10464=CARTESIAN_POINT('Ctrl Pts',(0.27570015339368,-1.4152837823473,0.618237860411764));
#10465=CARTESIAN_POINT('Ctrl Pts',(0.27570015339368,-1.4152837823473,0.618237860411764));
#10466=CARTESIAN_POINT('Ctrl Pts',(1.35277799022997,-1.62098550016515,0.617200513836093));
#10467=CARTESIAN_POINT('Ctrl Pts',(3.53092277948893,-1.89162724517065,0.615818637525046));
#10468=CARTESIAN_POINT('Ctrl Pts',(7.35893161235257,-1.96044797105896,0.61550283428964));
#10469=CARTESIAN_POINT('Ctrl Pts',(10.0753786444688,-1.75377172884558,0.616473434532366));
#10470=CARTESIAN_POINT('Ctrl Pts',(11.6974038588243,-1.59451504727786,0.617085749108931));
#10471=CARTESIAN_POINT('Ctrl Pts',(11.6681436286308,-1.2964346619681,0.9));
#10472=CARTESIAN_POINT('Ctrl Pts',(10.0505146497799,-1.45522470190849,0.9));
#10473=CARTESIAN_POINT('Ctrl Pts',(7.34698379851713,-1.66064017564263,0.9));
#10474=CARTESIAN_POINT('Ctrl Pts',(3.5507249968367,-1.5921338472202,0.9));
#10475=CARTESIAN_POINT('Ctrl Pts',(1.39628032950236,-1.32437289587156,0.9));
#10476=CARTESIAN_POINT('Ctrl Pts',(0.331856371369199,-1.12115139781563,
0.9));
#10477=CARTESIAN_POINT('Ctrl Pts',(12.0003454972153,-1.32890342861544,-0.00659247958978532));
#10478=CARTESIAN_POINT('Ctrl Pts',(11.9894744951615,-1.31808026232082,0.200838596530835));
#10479=CARTESIAN_POINT('Ctrl Pts',(11.9786034924455,-1.30725733885828,0.408269685287046));
#10480=CARTESIAN_POINT('Ctrl Pts',(11.9677324890572,-1.2964346619681,0.615700786872884));
#10481=CARTESIAN_POINT('Ctrl Pts',(12.000116620981,-1.41283311850955,-0.00222526087931226));
#10482=CARTESIAN_POINT('Ctrl Pts',(11.9892453109784,-1.40200002127642,0.205205215027088));
#10483=CARTESIAN_POINT('Ctrl Pts',(11.9783750177566,-1.39116761830557,0.412635780645844));
#10484=CARTESIAN_POINT('Ctrl Pts',(11.9675037034976,-1.38033490526933,0.620066275407343));
#10485=CARTESIAN_POINT('Ctrl Pts',(11.9341774721098,-1.5584705948029,0.00191796595980313));
#10486=CARTESIAN_POINT('Ctrl Pts',(11.9233226835938,-1.54762133657986,0.209348350794306));
#10487=CARTESIAN_POINT('Ctrl Pts',(11.9124678718222,-1.53677206634062,0.416778732304926));
#10488=CARTESIAN_POINT('Ctrl Pts',(11.9016132473252,-1.52592301942363,0.624209134118803));
#10489=CARTESIAN_POINT('Ctrl Pts',(11.7925116537096,-1.62071287545028,-0.0022587989925734));
#10490=CARTESIAN_POINT('Ctrl Pts',(11.7816834491585,-1.6098745265243,0.205173499361722));
#10491=CARTESIAN_POINT('Ctrl Pts',(11.7708551999607,-1.59903658749835,0.41260581547062));
#10492=CARTESIAN_POINT('Ctrl Pts',(11.760027440985,-1.58819854843564,0.620038149897102));
#10493=CARTESIAN_POINT('Ctrl Pts',(11.7298629188572,-1.62699926142283,-0.0052140742384003));
#10494=CARTESIAN_POINT('Ctrl Pts',(11.7190429637906,-1.61617098622686,0.202219177289036));
#10495=CARTESIAN_POINT('Ctrl Pts',(11.708223275703,-1.60534291388117,0.409652451626141));
#10496=CARTESIAN_POINT('Ctrl Pts',(11.6974038588243,-1.59451504727786,0.617085749108931));
#10497=CARTESIAN_POINT('Ctrl Pts',(12.,-1.32855945177638,-1.94722710178397E-16));
#10498=CARTESIAN_POINT('Ctrl Pts',(11.9892441636707,-1.31785094954632,0.205233583190348));
#10499=CARTESIAN_POINT('Ctrl Pts',(11.978488326693,-1.30714268506935,0.410467178751997));
#10500=CARTESIAN_POINT('Ctrl Pts',(11.9677324890572,-1.2964346619681,0.615700786872884));
#10501=CARTESIAN_POINT('Ctrl Pts',(11.6974038588243,-1.59451504727786,0.617085749108931));
#10502=CARTESIAN_POINT('Ctrl Pts',(11.7081326228587,-1.605252190239,0.41139047675572));
#10503=CARTESIAN_POINT('Ctrl Pts',(11.7188616535763,-1.61598953550924,0.205695227161956));
#10504=CARTESIAN_POINT('Ctrl Pts',(11.7295909468525,-1.62672708026858,8.73866951023317E-17));
#10505=CARTESIAN_POINT('Ctrl Pts',(11.7298546566854,1.62699099289774,-0.00505567716946009));
#10506=CARTESIAN_POINT('Ctrl Pts',(11.719037455812,1.61616547398006,0.202324775346606));
#10507=CARTESIAN_POINT('Ctrl Pts',(11.7082205217827,1.60534015781013,0.409705250660816));
#10508=CARTESIAN_POINT('Ctrl Pts',(11.6974038588243,1.59451504727786,0.617085749108931));
#10509=CARTESIAN_POINT('Ctrl Pts',(11.8133862946664,1.61860913476435,-0.00111531114554236));
#10510=CARTESIAN_POINT('Ctrl Pts',(11.8025579038448,1.6077699189899,0.206263846261978));
#10511=CARTESIAN_POINT('Ctrl Pts',(11.7917299466398,1.59693199028804,0.41364309356145));
#10512=CARTESIAN_POINT('Ctrl Pts',(11.7809019683719,1.58609304882157,0.621022283493159));
#10513=CARTESIAN_POINT('Ctrl Pts',(11.9519653779615,1.53884931758497,0.00198566945999789));
#10514=CARTESIAN_POINT('Ctrl Pts',(11.9411087765487,1.52800449744246,0.209363119024413));
#10515=CARTESIAN_POINT('Ctrl Pts',(11.9302521502216,1.51715965702667,0.416740564833343));
#10516=CARTESIAN_POINT('Ctrl Pts',(11.9193956662674,1.50631506689811,0.624118030142866));
#10517=CARTESIAN_POINT('Ctrl Pts',(12.0001655389052,1.39184242582033,-0.00315867047762133));
#10518=CARTESIAN_POINT('Ctrl Pts',(11.9892972278067,1.38101476165208,0.204219175612729));
#10519=CARTESIAN_POINT('Ctrl Pts',(11.9784292129672,1.37018709651964,0.41159703650799));
#10520=CARTESIAN_POINT('Ctrl Pts',(11.9675608998875,1.35935984444403,0.618974903273729));
#10521=CARTESIAN_POINT('Ctrl Pts',(12.0003371960637,1.32889516399154,-0.00643408418199817));
#10522=CARTESIAN_POINT('Ctrl Pts',(11.9894689610601,1.31807475269516,0.200944193475792));
#10523=CARTESIAN_POINT('Ctrl Pts',(11.9786007253947,1.3072545841082,0.408322483762789));
#10524=CARTESIAN_POINT('Ctrl Pts',(11.9677324890572,1.2964346619681,0.615700786872884));
#10525=CARTESIAN_POINT('Ctrl Pts',(11.7295909468525,1.62672708026857,-8.50014503228635E-17));
#10526=CARTESIAN_POINT('Ctrl Pts',(11.7188616535763,1.61598953550924,0.205695227161956));
#10527=CARTESIAN_POINT('Ctrl Pts',(11.7081326228587,1.605252190239,0.411390476755719));
#10528=CARTESIAN_POINT('Ctrl Pts',(11.6974038588243,1.59451504727786,0.617085749108931));
#10529=CARTESIAN_POINT('Ctrl Pts',(11.9677324890572,1.2964346619681,0.615700786872884));
#10530=CARTESIAN_POINT('Ctrl Pts',(11.978488326693,1.30714268506935,0.410467178751997));
#10531=CARTESIAN_POINT('Ctrl Pts',(11.9892441636707,1.31785094954633,0.205233583190349));
#10532=CARTESIAN_POINT('Ctrl Pts',(12.,1.32855945177638,-2.38524477946811E-17));
#10533=CARTESIAN_POINT('Ctrl Pts',(0.3318563713692,1.12115139781563,0.9));
#10534=CARTESIAN_POINT('Ctrl Pts',(1.92849230856897,1.42598364489954,0.9));
#10535=CARTESIAN_POINT('Ctrl Pts',(5.71993880054687,1.76935652211139,0.9));
#10536=CARTESIAN_POINT('Ctrl Pts',(9.51130499016288,1.50815471522196,0.9));
#10537=CARTESIAN_POINT('Ctrl Pts',(11.6681436286308,1.2964346619681,0.9));
#10538=CARTESIAN_POINT('Ctrl Pts',(0.315675209020018,1.2059043252356,0.9));
#10539=CARTESIAN_POINT('Ctrl Pts',(1.91774960754439,1.51208293277137,0.900011072182198));
#10540=CARTESIAN_POINT('Ctrl Pts',(5.72069615836457,1.85663493780214,0.899990666655967));
#10541=CARTESIAN_POINT('Ctrl Pts',(9.5180705084307,1.59456947801794,0.900005849269565));
#10542=CARTESIAN_POINT('Ctrl Pts',(11.6765943959699,1.38252448313292,0.9));
#10543=CARTESIAN_POINT('Ctrl Pts',(0.287623587302861,1.35283178372728,0.83061654407248));
#10544=CARTESIAN_POINT('Ctrl Pts',(1.89907070881462,1.6612970673762,0.830110312711064));
#10545=CARTESIAN_POINT('Ctrl Pts',(5.72203120258494,2.00791989451774,0.829536565111056));
#10546=CARTESIAN_POINT('Ctrl Pts',(9.52981562096212,1.74434245945332,0.829975639897288));
#10547=CARTESIAN_POINT('Ctrl Pts',(11.6912432102654,1.53175516862908,0.830242007927395));
#10548=CARTESIAN_POINT('Ctrl Pts',(0.276437927844243,1.41141950219787,0.682830994206899));
#10549=CARTESIAN_POINT('Ctrl Pts',(1.89175654834445,1.7202459032803,0.681514651829601));
#10550=CARTESIAN_POINT('Ctrl Pts',(5.72254254462207,2.06699613896002,0.680031275065471));
#10551=CARTESIAN_POINT('Ctrl Pts',(9.53442784766217,1.80334383841306,0.681166806353567));
#10552=CARTESIAN_POINT('Ctrl Pts',(11.6970428895979,1.59083777456472,0.681858145263204));
#10553=CARTESIAN_POINT('Ctrl Pts',(0.275700153393682,1.4152837823473,0.618237860411764));
#10554=CARTESIAN_POINT('Ctrl Pts',(1.89131690864814,1.72383635907408,0.616681840548257));
#10555=CARTESIAN_POINT('Ctrl Pts',(5.72257555688819,2.07025489722917,0.614922376024419));
#10556=CARTESIAN_POINT('Ctrl Pts',(9.53470357301702,1.80685728936816,0.616269329673511));
#10557=CARTESIAN_POINT('Ctrl Pts',(11.6974038588243,1.59451504727786,0.617085749108931));
#10558=CARTESIAN_POINT('Ctrl Pts',(11.6974038588243,1.59451504727786,0.617085749108931));
#10559=CARTESIAN_POINT('Ctrl Pts',(9.53470357301702,1.80685728936816,0.616269329673511));
#10560=CARTESIAN_POINT('Ctrl Pts',(5.72257555688819,2.07025489722917,0.614922376024419));
#10561=CARTESIAN_POINT('Ctrl Pts',(1.89131690864814,1.72383635907408,0.616681840548257));
#10562=CARTESIAN_POINT('Ctrl Pts',(0.275700153393682,1.4152837823473,0.618237860411764));
#10563=CARTESIAN_POINT('Ctrl Pts',(0.3318563713692,1.12115139781563,0.9));
#10564=CARTESIAN_POINT('Ctrl Pts',(1.92849230856897,1.42598364489954,0.9));
#10565=CARTESIAN_POINT('Ctrl Pts',(5.71993880054687,1.76935652211139,0.9));
#10566=CARTESIAN_POINT('Ctrl Pts',(9.51130499016288,1.50815471522196,0.9));
#10567=CARTESIAN_POINT('Ctrl Pts',(11.6681436286308,1.2964346619681,0.9));
#10568=CARTESIAN_POINT('Ctrl Pts',(-0.000343174493958709,1.15350944952984,
-0.00654815942696785));
#10569=CARTESIAN_POINT('Ctrl Pts',(0.0105270529019337,1.14272303380391,
0.200868135340743));
#10570=CARTESIAN_POINT('Ctrl Pts',(0.0213972813757523,1.13193701467556,
0.408284450676511));
#10571=CARTESIAN_POINT('Ctrl Pts',(0.0322675109428289,1.12115139781563,
0.615700786872884));
#10572=CARTESIAN_POINT('Ctrl Pts',(-0.000129060241737355,1.23228777111366,
-0.0024626161135415));
#10573=CARTESIAN_POINT('Ctrl Pts',(0.0107416412387167,1.22148297235423,
0.204952596860618));
#10574=CARTESIAN_POINT('Ctrl Pts',(0.0216107531875107,1.21067920461451,
0.412367946918899));
#10575=CARTESIAN_POINT('Ctrl Pts',(0.0324814606290031,1.19987501734845,
0.61978319007907));
#10576=CARTESIAN_POINT('Ctrl Pts',(0.0574602827844584,1.36931747586956,
0.00164530659801973));
#10577=CARTESIAN_POINT('Ctrl Pts',(0.0683025556324749,1.35848226928888,
0.209060253413207));
#10578=CARTESIAN_POINT('Ctrl Pts',(0.079145272670006,1.34764679267913,0.416475160658282));
#10579=CARTESIAN_POINT('Ctrl Pts',(0.0899872847341513,1.33681188280878,
0.62389013300849));
#10580=CARTESIAN_POINT('Ctrl Pts',(0.185325846363896,1.43651931939441,-0.00156109881554352));
#10581=CARTESIAN_POINT('Ctrl Pts',(0.196119220517603,1.4256988926218,0.205857093047737));
#10582=CARTESIAN_POINT('Ctrl Pts',(0.20691256009293,1.41487906031557,0.413275315721495));
#10583=CARTESIAN_POINT('Ctrl Pts',(0.217705180746507,1.40405902353128,0.620693562444772));
#10584=CARTESIAN_POINT('Ctrl Pts',(0.243371723604776,1.44769625339383,-0.00402191236404));
#10585=CARTESIAN_POINT('Ctrl Pts',(0.254148334883323,1.43689183478419,0.203397976373256));
#10586=CARTESIAN_POINT('Ctrl Pts',(0.264924480472538,1.42608767680315,0.410817900476086));
#10587=CARTESIAN_POINT('Ctrl Pts',(0.275700153393682,1.4152837823473,0.618237860411764));
#10588=CARTESIAN_POINT('Ctrl Pts',(-1.23734572934908E-17,1.15316892111333,
-8.67361737988404E-19));
#10589=CARTESIAN_POINT('Ctrl Pts',(0.0107558359204753,1.14249602316336,
0.205233575389367));
#10590=CARTESIAN_POINT('Ctrl Pts',(0.0215116728964674,1.13182351356624,
0.410467170919192));
#10591=CARTESIAN_POINT('Ctrl Pts',(0.0322675109428289,1.12115139781563,
0.615700786872884));
#10592=CARTESIAN_POINT('Ctrl Pts',(0.275700153393682,1.4152837823473,0.618237860411764));
#10593=CARTESIAN_POINT('Ctrl Pts',(0.264994127943615,1.42601784692504,0.412158538389472));
#10594=CARTESIAN_POINT('Ctrl Pts',(0.254287635915814,1.43675217163244,0.206079251738322));
#10595=CARTESIAN_POINT('Ctrl Pts',(0.243580684154575,1.44748675362873,-1.9298798670242E-17));
#10596=CARTESIAN_POINT('Ctrl Pts',(11.7295909468525,-1.62672708026858,0.));
#10597=CARTESIAN_POINT('Ctrl Pts',(11.7192775324813,-1.61592692249094,0.206079286804135));
#10598=CARTESIAN_POINT('Ctrl Pts',(11.70896411811,-1.6051267647133,0.41215857360827));
#10599=CARTESIAN_POINT('Ctrl Pts',(11.6986507037388,-1.59432660693566,0.618237860412405));
#10600=CARTESIAN_POINT('Ctrl Pts',(7.90092085928651,-2.00057770191527,0.));
#10601=CARTESIAN_POINT('Ctrl Pts',(7.89749915175266,-1.98977754413763,0.206079286804135));
#10602=CARTESIAN_POINT('Ctrl Pts',(7.89407744421881,-1.97897738636,0.41215857360827));
#10603=CARTESIAN_POINT('Ctrl Pts',(7.89065573668496,-1.96817722858236,0.618237860412405));
#10604=CARTESIAN_POINT('Ctrl Pts',(4.07225077172054,-2.17467835246083,0.));
#10605=CARTESIAN_POINT('Ctrl Pts',(4.07572077102407,-2.16387819468319,0.206079286804135));
#10606=CARTESIAN_POINT('Ctrl Pts',(4.07919077032759,-2.15307803690555,0.41215857360827));
#10607=CARTESIAN_POINT('Ctrl Pts',(4.08266076963111,-2.14227787912792,0.618237860412405));
#10608=CARTESIAN_POINT('Ctrl Pts',(0.243580684154574,-1.44748675362873,
0.));
#10609=CARTESIAN_POINT('Ctrl Pts',(0.253942390295469,-1.43668659585109,
0.206079286804135));
#10610=CARTESIAN_POINT('Ctrl Pts',(0.264304096436365,-1.42588643807345,
0.41215857360827));
#10611=CARTESIAN_POINT('Ctrl Pts',(0.27466580257726,-1.41508628029581,0.618237860412405));
#10612=CARTESIAN_POINT('Origin',(0.,-1.4,0.));
#10613=CARTESIAN_POINT('Origin',(6.08012166120517,1.06803409199199E-16,
0.9));
#10614=CARTESIAN_POINT('Ctrl Pts',(0.243580684154574,1.44748675362873,0.));
#10615=CARTESIAN_POINT('Ctrl Pts',(0.253942390295469,1.43668659585109,0.206079286804135));
#10616=CARTESIAN_POINT('Ctrl Pts',(0.264304096436365,1.42588643807345,0.41215857360827));
#10617=CARTESIAN_POINT('Ctrl Pts',(0.27466580257726,1.41508628029581,0.618237860412405));
#10618=CARTESIAN_POINT('Ctrl Pts',(4.07225077172054,2.17467835246083,0.));
#10619=CARTESIAN_POINT('Ctrl Pts',(4.07572077102407,2.16387819468319,0.206079286804135));
#10620=CARTESIAN_POINT('Ctrl Pts',(4.07919077032759,2.15307803690555,0.41215857360827));
#10621=CARTESIAN_POINT('Ctrl Pts',(4.08266076963111,2.14227787912792,0.618237860412405));
#10622=CARTESIAN_POINT('Ctrl Pts',(7.90092085928651,2.00057770191527,0.));
#10623=CARTESIAN_POINT('Ctrl Pts',(7.89749915175266,1.98977754413763,0.206079286804135));
#10624=CARTESIAN_POINT('Ctrl Pts',(7.89407744421881,1.97897738636,0.41215857360827));
#10625=CARTESIAN_POINT('Ctrl Pts',(7.89065573668496,1.96817722858236,0.618237860412405));
#10626=CARTESIAN_POINT('Ctrl Pts',(11.7295909468525,1.62672708026858,0.));
#10627=CARTESIAN_POINT('Ctrl Pts',(11.7192775324813,1.61592692249094,0.206079286804135));
#10628=CARTESIAN_POINT('Ctrl Pts',(11.70896411811,1.6051267647133,0.41215857360827));
#10629=CARTESIAN_POINT('Ctrl Pts',(11.6986507037388,1.59432660693566,0.618237860412405));
#10630=CARTESIAN_POINT('Origin',(12.,1.6,0.));
#10631=CARTESIAN_POINT('',(0.,0.,0.));
#10632=CARTESIAN_POINT('Origin',(9.,-1.,0.8));
#10633=CARTESIAN_POINT('',(8.85,-1.,0.9));
#10634=CARTESIAN_POINT('Origin',(9.,-1.,0.9));
#10635=CARTESIAN_POINT('',(8.85,-1.,0.7));
#10636=CARTESIAN_POINT('',(8.85,-1.,0.8));
#10637=CARTESIAN_POINT('Origin',(9.,-1.,0.7));
#10638=CARTESIAN_POINT('Origin',(3.,-1.,0.8));
#10639=CARTESIAN_POINT('',(2.85,-1.,0.9));
#10640=CARTESIAN_POINT('Origin',(3.,-1.,0.9));
#10641=CARTESIAN_POINT('',(2.85,-1.,0.7));
#10642=CARTESIAN_POINT('',(2.85,-1.,0.8));
#10643=CARTESIAN_POINT('Origin',(3.,-1.,0.7));
#10644=CARTESIAN_POINT('Origin',(3.,1.,0.8));
#10645=CARTESIAN_POINT('',(2.85,1.,0.9));
#10646=CARTESIAN_POINT('Origin',(3.,1.,0.9));
#10647=CARTESIAN_POINT('',(2.85,1.,0.7));
#10648=CARTESIAN_POINT('',(2.85,1.,0.8));
#10649=CARTESIAN_POINT('Origin',(3.,1.,0.7));
#10650=CARTESIAN_POINT('Origin',(9.,1.,0.8));
#10651=CARTESIAN_POINT('',(8.85,1.,0.9));
#10652=CARTESIAN_POINT('Origin',(9.,1.,0.9));
#10653=CARTESIAN_POINT('',(8.85,1.,0.7));
#10654=CARTESIAN_POINT('',(8.85,1.,0.8));
#10655=CARTESIAN_POINT('Origin',(9.,1.,0.7));
#10656=CARTESIAN_POINT('Origin',(10.1732050807569,0.3,0.9));
#10657=CARTESIAN_POINT('',(10.1732050807569,0.3,0.9));
#10658=CARTESIAN_POINT('',(10.3464101615138,0.,0.9));
#10659=CARTESIAN_POINT('',(9.72652155859676,1.07367855528516,0.9));
#10660=CARTESIAN_POINT('',(10.1732050807569,0.3,0.6));
#10661=CARTESIAN_POINT('',(10.1732050807569,0.3,0.9));
#10662=CARTESIAN_POINT('',(10.3464101615138,0.,0.6));
#10663=CARTESIAN_POINT('',(10.3464101615138,0.,0.6));
#10664=CARTESIAN_POINT('',(10.3464101615138,0.,0.9));
#10665=CARTESIAN_POINT('Origin',(9.82679491924311,0.3,0.9));
#10666=CARTESIAN_POINT('',(9.82679491924311,0.3,0.9));
#10667=CARTESIAN_POINT('',(7.95345829022414,0.3,0.9));
#10668=CARTESIAN_POINT('',(9.82679491924311,0.3,0.6));
#10669=CARTESIAN_POINT('',(9.82679491924311,0.3,0.9));
#10670=CARTESIAN_POINT('',(10.1732050807569,0.3,0.6));
#10671=CARTESIAN_POINT('Origin',(9.65358983848622,5.55111512312578E-17,
0.9));
#10672=CARTESIAN_POINT('',(9.65358983848622,4.24230095489963E-17,0.9));
#10673=CARTESIAN_POINT('',(9.2069063163261,-0.773678555285165,0.9));
#10674=CARTESIAN_POINT('',(9.65358983848622,5.55111512312578E-17,0.6));
#10675=CARTESIAN_POINT('',(9.65358983848622,4.24230095489963E-17,0.9));
#10676=CARTESIAN_POINT('',(9.82679491924311,0.3,0.6));
#10677=CARTESIAN_POINT('Origin',(9.82679491924311,-0.3,0.9));
#10678=CARTESIAN_POINT('',(9.82679491924311,-0.3,0.9));
#10679=CARTESIAN_POINT('',(9.29350885670454,0.623678555285165,0.9));
#10680=CARTESIAN_POINT('',(9.82679491924311,-0.3,0.6));
#10681=CARTESIAN_POINT('',(9.82679491924311,-0.3,0.9));
#10682=CARTESIAN_POINT('',(9.65358983848622,4.24230095489963E-17,0.6));
#10683=CARTESIAN_POINT('Origin',(10.1732050807569,-0.3,0.9));
#10684=CARTESIAN_POINT('',(10.1732050807569,-0.3,0.9));
#10685=CARTESIAN_POINT('',(8.12666337098103,-0.3,0.9));
#10686=CARTESIAN_POINT('',(10.1732050807569,-0.3,0.6));
#10687=CARTESIAN_POINT('',(10.1732050807569,-0.3,0.9));
#10688=CARTESIAN_POINT('',(9.82679491924311,-0.3,0.6));
#10689=CARTESIAN_POINT('Origin',(10.3464101615138,0.,0.9));
#10690=CARTESIAN_POINT('',(9.8131240989752,-0.923678555285165,0.9));
#10691=CARTESIAN_POINT('',(10.1732050807569,-0.3,0.6));
#10692=CARTESIAN_POINT('Origin',(10.,5.55111512312578E-17,0.6));
#10693=CARTESIAN_POINT('',(9.83,-2.0818995585505E-17,0.6));
#10694=CARTESIAN_POINT('Origin',(10.,0.,0.6));
#10695=CARTESIAN_POINT('Origin',(2.17320508075689,0.3,0.9));
#10696=CARTESIAN_POINT('',(2.17320508075689,0.3,0.9));
#10697=CARTESIAN_POINT('',(2.34641016151378,0.,0.9));
#10698=CARTESIAN_POINT('',(2.72652155859676,-0.65837225228371,0.9));
#10699=CARTESIAN_POINT('',(2.17320508075689,0.3,0.6));
#10700=CARTESIAN_POINT('',(2.17320508075689,0.3,0.9));
#10701=CARTESIAN_POINT('',(2.34641016151378,0.,0.6));
#10702=CARTESIAN_POINT('',(2.34641016151378,0.,0.6));
#10703=CARTESIAN_POINT('',(2.34641016151378,0.,0.9));
#10704=CARTESIAN_POINT('Origin',(1.82679491924311,0.3,0.9));
#10705=CARTESIAN_POINT('',(1.82679491924311,0.3,0.9));
#10706=CARTESIAN_POINT('',(3.95345829022414,0.3,0.9));
#10707=CARTESIAN_POINT('',(1.82679491924311,0.3,0.6));
#10708=CARTESIAN_POINT('',(1.82679491924311,0.3,0.9));
#10709=CARTESIAN_POINT('',(2.17320508075689,0.3,0.6));
#10710=CARTESIAN_POINT('Origin',(1.65358983848622,5.55111512312578E-17,
0.9));
#10711=CARTESIAN_POINT('',(1.65358983848622,4.24230095489963E-17,0.9));
#10712=CARTESIAN_POINT('',(2.20690631632609,0.958372252283711,0.9));
#10713=CARTESIAN_POINT('',(1.65358983848622,5.55111512312578E-17,0.6));
#10714=CARTESIAN_POINT('',(1.65358983848622,4.24230095489963E-17,0.9));
#10715=CARTESIAN_POINT('',(1.82679491924311,0.3,0.6));
#10716=CARTESIAN_POINT('Origin',(1.82679491924311,-0.3,0.9));
#10717=CARTESIAN_POINT('',(1.82679491924311,-0.3,0.9));
#10718=CARTESIAN_POINT('',(2.29350885670453,-1.10837225228371,0.9));
#10719=CARTESIAN_POINT('',(1.82679491924311,-0.3,0.6));
#10720=CARTESIAN_POINT('',(1.82679491924311,-0.3,0.9));
#10721=CARTESIAN_POINT('',(1.65358983848622,4.24230095489963E-17,0.6));
#10722=CARTESIAN_POINT('Origin',(2.17320508075689,-0.3,0.9));
#10723=CARTESIAN_POINT('',(2.17320508075689,-0.3,0.9));
#10724=CARTESIAN_POINT('',(4.12666337098103,-0.3,0.9));
#10725=CARTESIAN_POINT('',(2.17320508075689,-0.3,0.6));
#10726=CARTESIAN_POINT('',(2.17320508075689,-0.3,0.9));
#10727=CARTESIAN_POINT('',(1.82679491924311,-0.3,0.6));
#10728=CARTESIAN_POINT('Origin',(2.34641016151378,0.,0.9));
#10729=CARTESIAN_POINT('',(2.8131240989752,0.80837225228371,0.9));
#10730=CARTESIAN_POINT('',(2.17320508075689,-0.3,0.6));
#10731=CARTESIAN_POINT('Origin',(2.,5.55111512312578E-17,0.6));
#10732=CARTESIAN_POINT('',(1.83,-2.0818995585505E-17,0.6));
#10733=CARTESIAN_POINT('Origin',(2.,0.,0.6));
#10734=CARTESIAN_POINT('Origin',(2.,0.,0.45));
#10735=CARTESIAN_POINT('',(1.83,-2.0818995585505E-17,0.32));
#10736=CARTESIAN_POINT('',(1.83,2.0818995585505E-17,0.45));
#10737=CARTESIAN_POINT('Origin',(2.,0.,0.32));
#10738=CARTESIAN_POINT('Origin',(10.,0.,0.45));
#10739=CARTESIAN_POINT('',(9.83,-2.0818995585505E-17,0.32));
#10740=CARTESIAN_POINT('',(9.83,2.0818995585505E-17,0.45));
#10741=CARTESIAN_POINT('Origin',(10.,0.,0.32));
#10742=CARTESIAN_POINT('Origin',(11.2,-0.62,0.32));
#10743=CARTESIAN_POINT('',(0.200274469199584,-0.62,0.));
#10744=CARTESIAN_POINT('',(0.217044958570157,-0.62,0.32));
#10745=CARTESIAN_POINT('',(0.223426876981161,-0.62,0.441774257530303));
#10746=CARTESIAN_POINT('',(0.,-0.62,0.));
#10747=CARTESIAN_POINT('',(8.63987299740311,-0.62,0.));
#10748=CARTESIAN_POINT('',(0.0167704893705732,-0.62,0.32));
#10749=CARTESIAN_POINT('',(0.0237009700302462,-0.62,0.452241448778892));
#10750=CARTESIAN_POINT('',(-0.1,-0.62,0.32));
#10751=CARTESIAN_POINT('Origin',(11.2,-0.62,0.32));
#10752=CARTESIAN_POINT('',(0.9,-0.62,0.32));
#10753=CARTESIAN_POINT('',(0.9,-0.62,0.));
#10754=CARTESIAN_POINT('',(0.9,-0.62,0.16));
#10755=CARTESIAN_POINT('',(1.1,-0.62,0.32));
#10756=CARTESIAN_POINT('',(-0.1,-0.62,0.32));
#10757=CARTESIAN_POINT('',(1.1,-0.62,0.));
#10758=CARTESIAN_POINT('',(1.1,-0.62,0.16));
#10759=CARTESIAN_POINT('',(8.63987299740311,-0.62,0.));
#10760=CARTESIAN_POINT('Origin',(11.2,-0.62,0.32));
#10761=CARTESIAN_POINT('',(3.9,-0.62,0.32));
#10762=CARTESIAN_POINT('',(3.9,-0.62,0.));
#10763=CARTESIAN_POINT('',(3.9,-0.62,0.16));
#10764=CARTESIAN_POINT('',(4.1,-0.62,0.32));
#10765=CARTESIAN_POINT('',(-0.1,-0.62,0.32));
#10766=CARTESIAN_POINT('',(4.1,-0.62,0.));
#10767=CARTESIAN_POINT('',(4.1,-0.62,0.16));
#10768=CARTESIAN_POINT('',(8.63987299740311,-0.62,0.));
#10769=CARTESIAN_POINT('Origin',(11.2,-0.62,0.32));
#10770=CARTESIAN_POINT('',(7.9,-0.62,0.32));
#10771=CARTESIAN_POINT('',(7.9,-0.62,0.));
#10772=CARTESIAN_POINT('',(7.9,-0.62,0.16));
#10773=CARTESIAN_POINT('',(8.1,-0.62,0.32));
#10774=CARTESIAN_POINT('',(-0.1,-0.62,0.32));
#10775=CARTESIAN_POINT('',(8.1,-0.62,0.));
#10776=CARTESIAN_POINT('',(8.1,-0.62,0.16));
#10777=CARTESIAN_POINT('',(8.63987299740311,-0.62,0.));
#10778=CARTESIAN_POINT('Origin',(-0.0999999999999996,0.62,0.32));
#10779=CARTESIAN_POINT('',(0.217044958570158,0.62,0.32));
#10780=CARTESIAN_POINT('',(0.200274469199586,0.62,0.));
#10781=CARTESIAN_POINT('',(0.207951231396534,0.62,0.146481348799182));
#10782=CARTESIAN_POINT('',(0.0167704893705736,0.62,0.32));
#10783=CARTESIAN_POINT('',(11.2,0.62,0.32));
#10784=CARTESIAN_POINT('',(0.,0.62,0.));
#10785=CARTESIAN_POINT('',(0.00822532444561912,0.62,0.156948540047771));
#10786=CARTESIAN_POINT('',(2.98987299740311,0.62,0.));
#10787=CARTESIAN_POINT('Origin',(-0.0999999999999996,0.62,0.32));
#10788=CARTESIAN_POINT('',(0.9,0.62,0.));
#10789=CARTESIAN_POINT('',(0.9,0.62,0.32));
#10790=CARTESIAN_POINT('',(0.9,0.62,0.16));
#10791=CARTESIAN_POINT('',(1.1,0.62,0.));
#10792=CARTESIAN_POINT('',(2.98987299740311,0.62,0.));
#10793=CARTESIAN_POINT('',(1.1,0.62,0.32));
#10794=CARTESIAN_POINT('',(1.1,0.62,0.16));
#10795=CARTESIAN_POINT('',(11.2,0.62,0.32));
#10796=CARTESIAN_POINT('Origin',(-0.0999999999999996,0.62,0.32));
#10797=CARTESIAN_POINT('',(3.9,0.62,0.));
#10798=CARTESIAN_POINT('',(3.9,0.62,0.32));
#10799=CARTESIAN_POINT('',(3.9,0.62,0.16));
#10800=CARTESIAN_POINT('',(4.1,0.62,0.));
#10801=CARTESIAN_POINT('',(2.98987299740311,0.62,0.));
#10802=CARTESIAN_POINT('',(4.1,0.62,0.32));
#10803=CARTESIAN_POINT('',(4.1,0.62,0.16));
#10804=CARTESIAN_POINT('',(11.2,0.62,0.32));
#10805=CARTESIAN_POINT('Origin',(5.55,0.,0.32));
#10806=CARTESIAN_POINT('',(1.6,-4.89858719658941E-17,0.32));
#10807=CARTESIAN_POINT('Origin',(2.,0.,0.32));
#10808=CARTESIAN_POINT('Origin',(5.55,0.,0.32));
#10809=CARTESIAN_POINT('',(9.6,-4.89858719658942E-17,0.32));
#10810=CARTESIAN_POINT('Origin',(10.,0.,0.32));
#10811=CARTESIAN_POINT('Origin',(5.55,0.,0.32));
#10812=CARTESIAN_POINT('',(0.217044958570157,-0.7,0.32));
#10813=CARTESIAN_POINT('',(0.0167704893705731,-0.7,0.32));
#10814=CARTESIAN_POINT('Origin',(5.55,0.,0.32));
#10815=CARTESIAN_POINT('',(0.9,0.724814814814815,0.32));
#10816=CARTESIAN_POINT('',(1.1,-0.724814814814815,0.32));
#10817=CARTESIAN_POINT('Origin',(5.55,0.,0.32));
#10818=CARTESIAN_POINT('',(3.9,0.883148148148148,0.32));
#10819=CARTESIAN_POINT('',(4.1,-0.883148148148148,0.32));
#10820=CARTESIAN_POINT('Origin',(5.55,0.,0.32));
#10821=CARTESIAN_POINT('',(7.9,0.62,0.32));
#10822=CARTESIAN_POINT('',(7.9,0.886851851851852,0.32));
#10823=CARTESIAN_POINT('',(8.1,0.62,0.32));
#10824=CARTESIAN_POINT('',(11.2,0.62,0.32));
#10825=CARTESIAN_POINT('',(8.1,-0.886851851851852,0.32));
#10826=CARTESIAN_POINT('Origin',(-0.0999999999999996,0.62,0.32));
#10827=CARTESIAN_POINT('',(7.9,0.62,0.));
#10828=CARTESIAN_POINT('',(7.9,0.62,0.16));
#10829=CARTESIAN_POINT('',(8.1,0.62,0.));
#10830=CARTESIAN_POINT('',(2.98987299740311,0.62,0.));
#10831=CARTESIAN_POINT('',(8.1,0.62,0.16));
#10832=CARTESIAN_POINT('Origin',(11.2,1.53779953703704,0.));
#10833=CARTESIAN_POINT('',(11.2,1.47592264243751,0.));
#10834=CARTESIAN_POINT('',(11.2,-1.47592264243751,0.));
#10835=CARTESIAN_POINT('',(11.2,1.53779953703704,0.));
#10836=CARTESIAN_POINT('',(11.2,-1.44160695250311,0.605635447211793));
#10837=CARTESIAN_POINT('Ctrl Pts',(11.2,-1.44160695250311,0.605635447211793));
#10838=CARTESIAN_POINT('Ctrl Pts',(11.2,-1.44733381480461,0.504614841520655));
#10839=CARTESIAN_POINT('Ctrl Pts',(11.2,-1.45305922122436,0.403593539811385));
#10840=CARTESIAN_POINT('Ctrl Pts',(11.2,-1.46449774781658,0.201715464978033));
#10841=CARTESIAN_POINT('Ctrl Pts',(11.2,-1.47021094199039,0.100857470386242));
#10842=CARTESIAN_POINT('Ctrl Pts',(11.2,-1.47592264243751,0.));
#10843=CARTESIAN_POINT('',(11.2,-1.3413305091784,0.7));
#10844=CARTESIAN_POINT('Ctrl Pts',(11.2,-1.34133050917871,0.7));
#10845=CARTESIAN_POINT('Ctrl Pts',(11.2,-1.34927184579059,0.7));
#10846=CARTESIAN_POINT('Ctrl Pts',(11.1999981201149,-1.35715077597425,0.699006225306896));
#10847=CARTESIAN_POINT('Ctrl Pts',(11.1999964866412,-1.36482619101963,0.697118463987577));
#10848=CARTESIAN_POINT('Ctrl Pts',(11.1999955714568,-1.36912648693643,0.696060810134936));
#10849=CARTESIAN_POINT('Ctrl Pts',(11.1999947385598,-1.37336294684024,0.694721504600825));
#10850=CARTESIAN_POINT('Ctrl Pts',(11.1999942054834,-1.37750904339755,0.693111246644731));
#10851=CARTESIAN_POINT('Ctrl Pts',(11.1999932489192,-1.38494889279378,0.690221763364053));
#10852=CARTESIAN_POINT('Ctrl Pts',(11.1999934335488,-1.39201911070639,0.686493604183975));
#10853=CARTESIAN_POINT('Ctrl Pts',(11.1999946360439,-1.39857284316731,0.682006025455124));
#10854=CARTESIAN_POINT('Ctrl Pts',(11.1999952980149,-1.40218065925828,0.679535622697003));
#10855=CARTESIAN_POINT('Ctrl Pts',(11.1999962427007,-1.40563167682227,0.676834205328214));
#10856=CARTESIAN_POINT('Ctrl Pts',(11.1999970766466,-1.40889738828709,0.673909521834337));
#10857=CARTESIAN_POINT('Ctrl Pts',(11.1999978839828,-1.41205889660265,0.671078159882768));
#10858=CARTESIAN_POINT('Ctrl Pts',(11.1999985961359,-1.41502771690814,0.668054510912379));
#10859=CARTESIAN_POINT('Ctrl Pts',(11.1999985943254,-1.41778154893794,0.664849526385156));
#10860=CARTESIAN_POINT('Ctrl Pts',(11.1999985909468,-1.42292039881534,0.658868793295219));
#10861=CARTESIAN_POINT('Ctrl Pts',(11.1999963776609,-1.42731355725865,0.652257958652517));
#10862=CARTESIAN_POINT('Ctrl Pts',(11.1999956369,-1.43089859237711,0.645180832176479));
#10863=CARTESIAN_POINT('Ctrl Pts',(11.1999955610412,-1.43126572346771,0.644456088045497));
#10864=CARTESIAN_POINT('Ctrl Pts',(11.1999954968237,-1.43162433912915,0.643726434786758));
#10865=CARTESIAN_POINT('Ctrl Pts',(11.1999954455063,-1.43197434355081,0.642992037678167));
#10866=CARTESIAN_POINT('Ctrl Pts',(11.1999949451572,-1.43538691836834,0.635831599341589));
#10867=CARTESIAN_POINT('Ctrl Pts',(11.1999960935741,-1.43794480573841,0.628305806294037));
#10868=CARTESIAN_POINT('Ctrl Pts',(11.1999977538348,-1.43959303921538,0.620581877990282));
#10869=CARTESIAN_POINT('Ctrl Pts',(11.1999988103007,-1.44064185190664,0.615666946856702));
#10870=CARTESIAN_POINT('Ctrl Pts',(11.1999999935832,-1.44132148083109,0.610671141596651));
#10871=CARTESIAN_POINT('Ctrl Pts',(11.1999999950647,-1.44160695392865,0.605635447210179));
#10872=CARTESIAN_POINT('',(11.2,1.34133050917871,0.7));
#10873=CARTESIAN_POINT('',(11.2,0.768899768518519,0.7));
#10874=CARTESIAN_POINT('',(11.2,1.44160695250311,0.605635447211793));
#10875=CARTESIAN_POINT('Ctrl Pts',(11.1999999950647,1.44160695392865,0.605635447210179));
#10876=CARTESIAN_POINT('Ctrl Pts',(11.1999999927383,1.44115867123275,0.613543073794128));
#10877=CARTESIAN_POINT('Ctrl Pts',(11.199997327584,1.43974095598264,0.62135504174347));
#10878=CARTESIAN_POINT('Ctrl Pts',(11.1999961426836,1.43743894790867,0.628911795513178));
#10879=CARTESIAN_POINT('Ctrl Pts',(11.1999954950047,1.43618064644969,0.633042395401645));
#10880=CARTESIAN_POINT('Ctrl Pts',(11.1999951984378,1.4346571631488,0.63709676955888));
#10881=CARTESIAN_POINT('Ctrl Pts',(11.1999953420225,1.43287614971348,0.641047046155727));
#10882=CARTESIAN_POINT('Ctrl Pts',(11.1999956050472,1.42961361303411,0.648283331988978));
#10883=CARTESIAN_POINT('Ctrl Pts',(11.1999975633633,1.42552584716917,0.655091209244077));
#10884=CARTESIAN_POINT('Ctrl Pts',(11.1999983488166,1.42067941835906,0.661308913390503));
#10885=CARTESIAN_POINT('Ctrl Pts',(11.1999985007599,1.41974189284539,0.662511707551344));
#10886=CARTESIAN_POINT('Ctrl Pts',(11.1999985958742,1.41877583892185,0.663692344451305));
#10887=CARTESIAN_POINT('Ctrl Pts',(11.1999985956185,1.41778154881703,0.664849526385225));
#10888=CARTESIAN_POINT('Ctrl Pts',(11.199998595152,1.41596832836708,0.666959801783445));
#10889=CARTESIAN_POINT('Ctrl Pts',(11.1999982799021,1.41406123008998,0.668992111776222));
#10890=CARTESIAN_POINT('Ctrl Pts',(11.1999978412043,1.41206657472189,0.670943322037058));
#10891=CARTESIAN_POINT('Ctrl Pts',(11.1999965906985,1.40638082038708,0.676505236328724));
#10892=CARTESIAN_POINT('Ctrl Pts',(11.1999945592311,1.40005057587654,0.681348449922958));
#10893=CARTESIAN_POINT('Ctrl Pts',(11.1999938793032,1.39324090595796,0.685420973467861));
#10894=CARTESIAN_POINT('Ctrl Pts',(11.1999934424014,1.38886521116801,0.68803785802621));
#10895=CARTESIAN_POINT('Ctrl Pts',(11.1999934711477,1.38429057260668,0.690335857752236));
#10896=CARTESIAN_POINT('Ctrl Pts',(11.1999939665515,1.37955471147715,0.692291686537622));
#10897=CARTESIAN_POINT('Ctrl Pts',(11.1999947349645,1.37220899016913,0.695325342464331));
#10898=CARTESIAN_POINT('Ctrl Pts',(11.1999966395725,1.36455954597093,0.697503651902993));
#10899=CARTESIAN_POINT('Ctrl Pts',(11.1999981885915,1.35675452105021,0.698758058199902));
#10900=CARTESIAN_POINT('Ctrl Pts',(11.1999991983045,1.35166689148409,0.699575730741489));
#10901=CARTESIAN_POINT('Ctrl Pts',(11.2,1.34651254223162,0.7));
#10902=CARTESIAN_POINT('Ctrl Pts',(11.2,1.34133050917871,0.7));
#10903=CARTESIAN_POINT('Ctrl Pts',(11.2,1.47592264243751,0.));
#10904=CARTESIAN_POINT('Ctrl Pts',(11.2,1.47021025951677,0.100869521536925));
#10905=CARTESIAN_POINT('Ctrl Pts',(11.2,1.4644963825062,0.20173956751342));
#10906=CARTESIAN_POINT('Ctrl Pts',(11.2,1.45305785520703,0.403617642353031));
#10907=CARTESIAN_POINT('Ctrl Pts',(11.2,1.44733313162379,0.50462689268162));
#10908=CARTESIAN_POINT('Ctrl Pts',(11.2,1.44160695250311,0.605635447211793));
#10909=CARTESIAN_POINT('Origin',(8.1,-1.7737037037037,0.));
#10910=CARTESIAN_POINT('',(8.1,1.69866351109718,0.));
#10911=CARTESIAN_POINT('',(8.1,-1.7737037037037,0.));
#10912=CARTESIAN_POINT('',(8.1,1.66641703131627,0.605314487869832));
#10913=CARTESIAN_POINT('Ctrl Pts',(8.1,1.66641703131627,0.605314487869832));
#10914=CARTESIAN_POINT('Ctrl Pts',(8.1,1.67178339996556,0.504592280948055));
#10915=CARTESIAN_POINT('Ctrl Pts',(8.1,1.67714947719849,0.403869246528492));
#10916=CARTESIAN_POINT('Ctrl Pts',(8.1,1.68789827452893,0.202098297941347));
#10917=CARTESIAN_POINT('Ctrl Pts',(8.1,1.69328107955938,0.101048748975501));
#10918=CARTESIAN_POINT('Ctrl Pts',(8.1,1.69866351109718,0.));
#10919=CARTESIAN_POINT('',(8.1,1.56644778183753,0.7));
#10920=CARTESIAN_POINT('Ctrl Pts',(8.0999999986552,1.56644778212326,0.7));
#10921=CARTESIAN_POINT('Ctrl Pts',(8.10000000155239,1.57436337254628,0.699999999341293));
#10922=CARTESIAN_POINT('Ctrl Pts',(8.09999905041684,1.58221543358893,0.699005989267703));
#10923=CARTESIAN_POINT('Ctrl Pts',(8.09999821745812,1.58986365929578,0.697118696434997));
#10924=CARTESIAN_POINT('Ctrl Pts',(8.099997748439,1.59417019217574,0.69605600700222));
#10925=CARTESIAN_POINT('Ctrl Pts',(8.09999731997616,1.59841215407948,0.694709061504878));
#10926=CARTESIAN_POINT('Ctrl Pts',(8.09999704681388,1.60256279759721,0.693088866918468));
#10927=CARTESIAN_POINT('Ctrl Pts',(8.09999655811104,1.60998853482381,0.690190246691698));
#10928=CARTESIAN_POINT('Ctrl Pts',(8.09999665589197,1.61704187682962,0.686451534538094));
#10929=CARTESIAN_POINT('Ctrl Pts',(8.09999726576867,1.62357667434142,0.681954089017224));
#10930=CARTESIAN_POINT('Ctrl Pts',(8.09999760196939,1.62717904774802,0.679474826559159));
#10931=CARTESIAN_POINT('Ctrl Pts',(8.09999808150314,1.6306235748906,0.676764109620253));
#10932=CARTESIAN_POINT('Ctrl Pts',(8.09999850764167,1.63388182210815,0.673830012183301));
#10933=CARTESIAN_POINT('Ctrl Pts',(8.09999892160867,1.637047006066,0.670979719520364));
#10934=CARTESIAN_POINT('Ctrl Pts',(8.09999928906958,1.640017230617,0.667935813742119));
#10935=CARTESIAN_POINT('Ctrl Pts',(8.09999928944056,1.64277007752663,0.664709670235875));
#10936=CARTESIAN_POINT('Ctrl Pts',(8.09999929012967,1.64788359851353,0.658716982277737));
#10937=CARTESIAN_POINT('Ctrl Pts',(8.09999816327153,1.65225000627493,0.652096887528603));
#10938=CARTESIAN_POINT('Ctrl Pts',(8.09999778355904,1.65580927004486,0.645014643130784));
#10939=CARTESIAN_POINT('Ctrl Pts',(8.09999774450894,1.65617530914943,0.644286296325024));
#10940=CARTESIAN_POINT('Ctrl Pts',(8.09999771143612,1.65653277094855,0.643553041785202));
#10941=CARTESIAN_POINT('Ctrl Pts',(8.0999976850083,1.65688156115921,0.642815048027137));
#10942=CARTESIAN_POINT('Ctrl Pts',(8.09999742811004,1.66027206465027,0.635641192980042));
#10943=CARTESIAN_POINT('Ctrl Pts',(8.09999800724182,1.66280786743682,0.628104262855387));
#10944=CARTESIAN_POINT('Ctrl Pts',(8.09999885110511,1.66443535430957,0.620372450280339));
#10945=CARTESIAN_POINT('Ctrl Pts',(8.09999939164969,1.6654778563549,0.615419764910946));
#10946=CARTESIAN_POINT('Ctrl Pts',(8.1,1.66614680274328,0.610386449940169));
#10947=CARTESIAN_POINT('Ctrl Pts',(8.1,1.66641703131627,0.605314487869832));
#10948=CARTESIAN_POINT('',(8.1,-1.56644778183827,0.7));
#10949=CARTESIAN_POINT('',(8.1,-0.886851851851852,0.7));
#10950=CARTESIAN_POINT('',(8.1,-1.66641703131627,0.605314487869832));
#10951=CARTESIAN_POINT('Ctrl Pts',(8.1,-1.66641703131627,0.605314487869832));
#10952=CARTESIAN_POINT('Ctrl Pts',(8.1,-1.66599546653325,0.613226902778437));
#10953=CARTESIAN_POINT('Ctrl Pts',(8.09999864563672,-1.66460605882141,0.621047760783158));
#10954=CARTESIAN_POINT('Ctrl Pts',(8.09999804140045,-1.66233302739118,0.628616817026045));
#10955=CARTESIAN_POINT('Ctrl Pts',(8.09999770486592,-1.66106704316887,0.632832467392296));
#10956=CARTESIAN_POINT('Ctrl Pts',(8.0999975536836,-1.65952595995304,0.636970042829054));
#10957=CARTESIAN_POINT('Ctrl Pts',(8.09999763427866,-1.65771765414013,0.640999885518982));
#10958=CARTESIAN_POINT('Ctrl Pts',(8.09999777898787,-1.65447082344915,0.64823550729937));
#10959=CARTESIAN_POINT('Ctrl Pts',(8.09999878245444,-1.65040085231772,0.655045563401426));
#10960=CARTESIAN_POINT('Ctrl Pts',(8.09999917121848,-1.64557198994432,0.661267087195486));
#10961=CARTESIAN_POINT('Ctrl Pts',(8.09999924425118,-1.6446648462537,0.662435854416292));
#10962=CARTESIAN_POINT('Ctrl Pts',(8.09999928944999,-1.64373079085321,0.663583781603691));
#10963=CARTESIAN_POINT('Ctrl Pts',(8.09999928890117,-1.64277007755202,0.664709670235858));
#10964=CARTESIAN_POINT('Ctrl Pts',(8.09999928782175,-1.64088054556816,0.666924069243459));
#10965=CARTESIAN_POINT('Ctrl Pts',(8.09999911129818,-1.63888792496677,0.66905326411728));
#10966=CARTESIAN_POINT('Ctrl Pts',(8.09999887085824,-1.63679941630975,0.671093569621172));
#10967=CARTESIAN_POINT('Ctrl Pts',(8.09999821641022,-1.6311147520694,0.676647030794692));
#10968=CARTESIAN_POINT('Ctrl Pts',(8.0999972000003,-1.62478663867955,0.681482189379454));
#10969=CARTESIAN_POINT('Ctrl Pts',(8.09999686812141,-1.6179789612855,0.685544965666037));
#10970=CARTESIAN_POINT('Ctrl Pts',(8.09999665686968,-1.61364565292072,0.68813105508359));
#10971=CARTESIAN_POINT('Ctrl Pts',(8.09999667786582,-1.6091170759025,0.690403516124292));
#10972=CARTESIAN_POINT('Ctrl Pts',(8.0999969341683,-1.60442977212996,0.692339085768374));
#10973=CARTESIAN_POINT('Ctrl Pts',(8.09999733452329,-1.59710801128849,0.695362524980696));
#10974=CARTESIAN_POINT('Ctrl Pts',(8.09999831212369,-1.58948382509795,0.697531565976904));
#10975=CARTESIAN_POINT('Ctrl Pts',(8.09999909563861,-1.58170429192971,0.698776637084609));
#10976=CARTESIAN_POINT('Ctrl Pts',(8.09999960249138,-1.57667174192468,0.69958206878261));
#10977=CARTESIAN_POINT('Ctrl Pts',(8.1000000005313,-1.5715735875011,0.699999999573449));
#10978=CARTESIAN_POINT('Ctrl Pts',(8.0999999986552,-1.56644778212326,0.7));
#10979=CARTESIAN_POINT('',(8.1,-1.69866351109718,0.));
#10980=CARTESIAN_POINT('Ctrl Pts',(8.1,-1.69866351109718,0.));
#10981=CARTESIAN_POINT('Ctrl Pts',(8.1,-1.69328105674055,0.101049177371948));
#10982=CARTESIAN_POINT('Ctrl Pts',(8.1,-1.68789822886868,0.202099155105557));
#10983=CARTESIAN_POINT('Ctrl Pts',(8.1,-1.67714943151225,0.403870104074094));
#10984=CARTESIAN_POINT('Ctrl Pts',(8.1,-1.67178337712185,0.50459270970527));
#10985=CARTESIAN_POINT('Ctrl Pts',(8.1,-1.66641703131627,0.605314487869832));
#10986=CARTESIAN_POINT('',(8.1,-1.7737037037037,0.));
#10987=CARTESIAN_POINT('Origin',(4.1,-1.7662962962963,0.));
#10988=CARTESIAN_POINT('',(4.1,1.70113889814581,0.));
#10989=CARTESIAN_POINT('',(4.1,-1.7662962962963,0.));
#10990=CARTESIAN_POINT('',(4.1,1.66887738702937,0.605315322680072));
#10991=CARTESIAN_POINT('Ctrl Pts',(4.1,1.66887738702937,0.605315322680072));
#10992=CARTESIAN_POINT('Ctrl Pts',(4.1,1.67424235111642,0.50466767694528));
#10993=CARTESIAN_POINT('Ctrl Pts',(4.1,1.67960699363804,0.404019058341251));
#10994=CARTESIAN_POINT('Ctrl Pts',(4.1,1.69036079691899,0.202247931921761));
#10995=CARTESIAN_POINT('Ctrl Pts',(4.1,1.6957500571643,0.101123491803998));
#10996=CARTESIAN_POINT('Ctrl Pts',(4.1,1.70113889814581,0.));
#10997=CARTESIAN_POINT('',(4.1,1.56887583540973,0.7));
#10998=CARTESIAN_POINT('Ctrl Pts',(4.1,1.56887583540973,0.7));
#10999=CARTESIAN_POINT('Ctrl Pts',(4.1,1.57679416129392,0.7));
#11000=CARTESIAN_POINT('Ctrl Pts',(4.10000107724674,1.58464912207822,0.699006028000541));
#11001=CARTESIAN_POINT('Ctrl Pts',(4.10000201939527,1.59230028572239,0.697118705459362));
#11002=CARTESIAN_POINT('Ctrl Pts',(4.10000255022779,1.59661116283941,0.696055335763773));
#11003=CARTESIAN_POINT('Ctrl Pts',(4.10000303435977,1.60085740028891,0.694707333985525));
#11004=CARTESIAN_POINT('Ctrl Pts',(4.10000334030352,1.60501217339351,0.693085708041268));
#11005=CARTESIAN_POINT('Ctrl Pts',(4.10000388718746,1.61243895913315,0.690187001388783));
#11006=CARTESIAN_POINT('Ctrl Pts',(4.10000376557609,1.61949349263125,0.686448444730844));
#11007=CARTESIAN_POINT('Ctrl Pts',(4.10000306534783,1.6260295229635,0.681951159450519));
#11008=CARTESIAN_POINT('Ctrl Pts',(4.10000267892397,1.62963645835533,0.679469313954069));
#11009=CARTESIAN_POINT('Ctrl Pts',(4.10000213012555,1.63308521926452,0.676755517937216));
#11010=CARTESIAN_POINT('Ctrl Pts',(4.1000016436875,1.63634725251217,0.673817835781739));
#11011=CARTESIAN_POINT('Ctrl Pts',(4.10000117237165,1.63950787692018,0.67097147916344));
#11012=CARTESIAN_POINT('Ctrl Pts',(4.10000075597222,1.64247408874941,0.667932078875657));
#11013=CARTESIAN_POINT('Ctrl Pts',(4.10000075698646,1.64522354659423,0.664710927554201));
#11014=CARTESIAN_POINT('Ctrl Pts',(4.1000007588733,1.65033845220459,0.658718515269377));
#11015=CARTESIAN_POINT('Ctrl Pts',(4.10000204656096,1.65470614797426,0.652098486008568));
#11016=CARTESIAN_POINT('Ctrl Pts',(4.10000248678323,1.65826650381873,0.645016049251367));
#11017=CARTESIAN_POINT('Ctrl Pts',(4.10000253228732,1.65863452415637,0.644283964909082));
#11018=CARTESIAN_POINT('Ctrl Pts',(4.10000257095464,1.65899387729575,0.643546919913709));
#11019=CARTESIAN_POINT('Ctrl Pts',(4.10000260201855,1.65934446736461,0.642805085364403));
#11020=CARTESIAN_POINT('Ctrl Pts',(4.10000290242009,1.66273482600052,0.635631222228741));
#11021=CARTESIAN_POINT('Ctrl Pts',(4.10000225562543,1.66527033938482,0.628094305374488));
#11022=CARTESIAN_POINT('Ctrl Pts',(4.10000130084992,1.66689736875237,0.62036252267401));
#11023=CARTESIAN_POINT('Ctrl Pts',(4.10000068968835,1.66793884687677,0.615413329558163));
#11024=CARTESIAN_POINT('Ctrl Pts',(4.09999999901039,1.66860722297681,0.610383627857512));
#11025=CARTESIAN_POINT('Ctrl Pts',(4.09999999630223,1.66887738567036,0.60531532268817));
#11026=CARTESIAN_POINT('',(4.1,-1.56887583540947,0.7));
#11027=CARTESIAN_POINT('',(4.1,-0.883148148148148,0.7));
#11028=CARTESIAN_POINT('',(4.1,-1.66887738702937,0.605315322680072));
#11029=CARTESIAN_POINT('Ctrl Pts',(4.09999999630223,-1.66887738567036,0.60531532268817));
#11030=CARTESIAN_POINT('Ctrl Pts',(4.10000000053001,-1.66845562780346,0.613227583070809));
#11031=CARTESIAN_POINT('Ctrl Pts',(4.10000153668442,-1.66706589531621,0.621048261667561));
#11032=CARTESIAN_POINT('Ctrl Pts',(4.10000221487211,-1.66479240287642,0.628617079688242));
#11033=CARTESIAN_POINT('Ctrl Pts',(4.10000259231836,-1.6635270876889,0.632829515245766));
#11034=CARTESIAN_POINT('Ctrl Pts',(4.10000275805793,-1.66198703315979,0.636963972243471));
#11035=CARTESIAN_POINT('Ctrl Pts',(4.10000266178038,-1.66018010017296,0.640990858692597));
#11036=CARTESIAN_POINT('Ctrl Pts',(4.10000248876893,-1.65693302887506,0.648227201990446));
#11037=CARTESIAN_POINT('Ctrl Pts',(4.10000134097948,-1.65286254930452,0.655037795911226));
#11038=CARTESIAN_POINT('Ctrl Pts',(4.100000893742,-1.6480330317196,0.661259713776781));
#11039=CARTESIAN_POINT('Ctrl Pts',(4.10000080951506,-1.647123502594,0.662431469633614));
#11040=CARTESIAN_POINT('Ctrl Pts',(4.10000075717637,-1.6461869221106,0.663582276554164));
#11041=CARTESIAN_POINT('Ctrl Pts',(4.10000075728519,-1.64522354661022,0.66471092755419));
#11042=CARTESIAN_POINT('Ctrl Pts',(4.10000075749815,-1.64333815989002,0.666919768869269));
#11043=CARTESIAN_POINT('Ctrl Pts',(4.1000009568795,-1.64135017761634,0.669043797975229));
#11044=CARTESIAN_POINT('Ctrl Pts',(4.10000122972053,-1.63926675509047,0.671079366787198));
#11045=CARTESIAN_POINT('Ctrl Pts',(4.10000197419082,-1.6335819569127,0.676633591976433));
#11046=CARTESIAN_POINT('Ctrl Pts',(4.10000313643093,-1.62725355063421,0.681469444454218));
#11047=CARTESIAN_POINT('Ctrl Pts',(4.1000035230587,-1.62044557755217,0.685533082105531));
#11048=CARTESIAN_POINT('Ctrl Pts',(4.10000376939409,-1.61610795658125,0.688122181633714));
#11049=CARTESIAN_POINT('Ctrl Pts',(4.10000375220654,-1.61157469281532,0.690397125746379));
#11050=CARTESIAN_POINT('Ctrl Pts',(4.10000346632868,-1.60688245467732,0.692334655286926));
#11051=CARTESIAN_POINT('Ctrl Pts',(4.10000302008581,-1.59955807566073,0.695359054367588));
#11052=CARTESIAN_POINT('Ctrl Pts',(4.1000019139068,-1.59193114173487,0.69752894708864));
#11053=CARTESIAN_POINT('Ctrl Pts',(4.10000102635309,-1.58414888227482,0.698774888159427));
#11054=CARTESIAN_POINT('Ctrl Pts',(4.10000045177616,-1.57911086966871,0.699581474839467));
#11055=CARTESIAN_POINT('Ctrl Pts',(4.1,-1.57400716417114,0.7));
#11056=CARTESIAN_POINT('Ctrl Pts',(4.1,-1.56887583540973,0.7));
#11057=CARTESIAN_POINT('',(4.1,-1.70113889814582,0.));
#11058=CARTESIAN_POINT('Ctrl Pts',(4.1,-1.70113889814582,0.));
#11059=CARTESIAN_POINT('Ctrl Pts',(4.1,-1.69575004793467,0.101123665001254));
#11060=CARTESIAN_POINT('Ctrl Pts',(4.1,-1.69036077845691,0.202248278345555));
#11061=CARTESIAN_POINT('Ctrl Pts',(4.1,-1.67960697517202,0.404019404791024));
#11062=CARTESIAN_POINT('Ctrl Pts',(4.1,-1.67424234188296,0.504667850166609));
#11063=CARTESIAN_POINT('Ctrl Pts',(4.1,-1.66887738702937,0.605315322680072));
#11064=CARTESIAN_POINT('',(4.1,-1.7662962962963,0.));
#11065=CARTESIAN_POINT('Origin',(1.1,-1.44962962962963,0.));
#11066=CARTESIAN_POINT('',(1.1,1.39262953588351,0.));
#11067=CARTESIAN_POINT('',(1.1,-1.44962962962963,0.));
#11068=CARTESIAN_POINT('',(1.10000000000005,1.35674377243284,0.605845626926786));
#11069=CARTESIAN_POINT('Ctrl Pts',(1.10000000000005,1.35674377243284,0.605845626926786));
#11070=CARTESIAN_POINT('Ctrl Pts',(1.10000000000005,1.36273568520883,0.504787121979256));
#11071=CARTESIAN_POINT('Ctrl Pts',(1.1,1.36872466312622,0.403727404115485));
#11072=CARTESIAN_POINT('Ctrl Pts',(1.1,1.38068651056748,0.201779555185378));
#11073=CARTESIAN_POINT('Ctrl Pts',(1.1,1.38665951284069,0.10088935150083));
#11074=CARTESIAN_POINT('Ctrl Pts',(1.1,1.39262953588351,0.));
#11075=CARTESIAN_POINT('',(1.1,1.25565664448622,0.7));
#11076=CARTESIAN_POINT('Ctrl Pts',(1.1,1.25565664448621,0.7));
#11077=CARTESIAN_POINT('Ctrl Pts',(1.1,1.26365753466764,0.700000000000001));
#11078=CARTESIAN_POINT('Ctrl Pts',(1.10000312127109,1.27160078819195,0.699008097631352));
#11079=CARTESIAN_POINT('Ctrl Pts',(1.10000579554281,1.27934333527045,0.697120485426804));
#11080=CARTESIAN_POINT('Ctrl Pts',(1.10000709386889,1.28310224676699,0.696204072889075));
#11081=CARTESIAN_POINT('Ctrl Pts',(1.10000828779753,1.28681383019745,0.695075712339665));
#11082=CARTESIAN_POINT('Ctrl Pts',(1.10000913303706,1.29046059826345,0.693742188764313));
#11083=CARTESIAN_POINT('Ctrl Pts',(1.10001087659788,1.29798315455626,0.69099139518989));
#11084=CARTESIAN_POINT('Ctrl Pts',(1.10001086910546,1.30515375246939,0.687398976275641));
#11085=CARTESIAN_POINT('Ctrl Pts',(1.10000899624477,1.31182501206943,0.683041610144935));
#11086=CARTESIAN_POINT('Ctrl Pts',(1.10000779407289,1.31610723164143,0.680244657298552));
#11087=CARTESIAN_POINT('Ctrl Pts',(1.10000585478529,1.32018349952736,0.677131483611404));
#11088=CARTESIAN_POINT('Ctrl Pts',(1.10000422180804,1.32400796947387,0.673713330684339));
#11089=CARTESIAN_POINT('Ctrl Pts',(1.10000291018178,1.3270798280974,0.670967830603965));
#11090=CARTESIAN_POINT('Ctrl Pts',(1.10000180047651,1.32997084712789,0.668041731908725));
#11091=CARTESIAN_POINT('Ctrl Pts',(1.10000182449184,1.33266034096938,0.664944387470286));
#11092=CARTESIAN_POINT('Ctrl Pts',(1.10000187074845,1.33784065079383,0.65897850512594));
#11093=CARTESIAN_POINT('Ctrl Pts',(1.10000564109429,1.34227630326151,0.652378581761819));
#11094=CARTESIAN_POINT('Ctrl Pts',(1.10000696187003,1.34590032739451,0.645305437365917));
#11095=CARTESIAN_POINT('Ctrl Pts',(1.100007110355,1.34630774940504,0.644510256482779));
#11096=CARTESIAN_POINT('Ctrl Pts',(1.10000723579819,1.34670486410349,0.643709073603569));
#11097=CARTESIAN_POINT('Ctrl Pts',(1.10000733566964,1.34709153749004,0.642902104572485));
#11098=CARTESIAN_POINT('Ctrl Pts',(1.10000822022419,1.35051627708745,0.63575483535061));
#11099=CARTESIAN_POINT('Ctrl Pts',(1.10000635568239,1.35308446649167,0.628241602461225));
#11100=CARTESIAN_POINT('Ctrl Pts',(1.10000361780323,1.35473867947858,0.620527690691125));
#11101=CARTESIAN_POINT('Ctrl Pts',(1.1000019043033,1.35577396762308,0.615699943921843));
#11102=CARTESIAN_POINT('Ctrl Pts',(1.09999998677418,1.35645041192828,0.610792997969602));
#11103=CARTESIAN_POINT('Ctrl Pts',(1.09999997754868,1.35674374570294,0.605845627052288));
#11104=CARTESIAN_POINT('',(1.1,-1.25565664448622,0.7));
#11105=CARTESIAN_POINT('',(1.1,-0.724814814814815,0.7));
#11106=CARTESIAN_POINT('',(1.10000000000005,-1.35674377243284,0.605845626926786));
#11107=CARTESIAN_POINT('Ctrl Pts',(1.09999997754868,-1.35674374570294,0.605845627052288));
#11108=CARTESIAN_POINT('Ctrl Pts',(1.09999999227748,-1.35627542940044,0.613744255356351));
#11109=CARTESIAN_POINT('Ctrl Pts',(1.1000044245081,-1.35483313756702,0.621542702113576));
#11110=CARTESIAN_POINT('Ctrl Pts',(1.10000632213307,-1.3525036790266,0.629082464357584));
#11111=CARTESIAN_POINT('Ctrl Pts',(1.1000073336739,-1.3512619466217,0.633101581650771));
#11112=CARTESIAN_POINT('Ctrl Pts',(1.10000777634458,-1.34976719347553,0.637047225321331));
#11113=CARTESIAN_POINT('Ctrl Pts',(1.10000752568741,-1.34802684471036,0.640893844816285));
#11114=CARTESIAN_POINT('Ctrl Pts',(1.10000705344834,-1.3447480208661,0.648140890909733));
#11115=CARTESIAN_POINT('Ctrl Pts',(1.10000374385205,-1.34063788586045,0.654954534019122));
#11116=CARTESIAN_POINT('Ctrl Pts',(1.10000230512149,-1.33576793982513,0.661175616324976));
#11117=CARTESIAN_POINT('Ctrl Pts',(1.10000200863552,-1.33476436716076,0.662457623989879));
#11118=CARTESIAN_POINT('Ctrl Pts',(1.10000181701501,-1.33372836971272,0.663714393476354));
#11119=CARTESIAN_POINT('Ctrl Pts',(1.10000180919237,-1.33266033853372,0.664944387472089));
#11120=CARTESIAN_POINT('Ctrl Pts',(1.10000179685332,-1.33097567746633,0.666884520904953));
#11121=CARTESIAN_POINT('Ctrl Pts',(1.10000223926429,-1.32921133126375,0.668758058859172));
#11122=CARTESIAN_POINT('Ctrl Pts',(1.10000288715521,-1.32737234926393,0.670562692084704));
#11123=CARTESIAN_POINT('Ctrl Pts',(1.10000489069569,-1.32168547392559,0.676143347135183));
#11124=CARTESIAN_POINT('Ctrl Pts',(1.10000845923633,-1.31535192007569,0.681005160308095));
#11125=CARTESIAN_POINT('Ctrl Pts',(1.1000097672184,-1.30853956043085,0.685101187995272));
#11126=CARTESIAN_POINT('Ctrl Pts',(1.10001062829021,-1.30405484229164,0.687797688271992));
#11127=CARTESIAN_POINT('Ctrl Pts',(1.10001067755751,-1.29936155475819,0.690161668140197));
#11128=CARTESIAN_POINT('Ctrl Pts',(1.10000992106221,-1.29450057597768,0.692169783635984));
#11129=CARTESIAN_POINT('Ctrl Pts',(1.10000876843985,-1.28709422081189,0.695229417764685));
#11130=CARTESIAN_POINT('Ctrl Pts',(1.100005676647,-1.27938091857402,0.69743146309387));
#11131=CARTESIAN_POINT('Ctrl Pts',(1.10000309801581,-1.2715114871423,0.698709794160748));
#11132=CARTESIAN_POINT('Ctrl Pts',(1.10000138449209,-1.26628217885177,0.699559256705032));
#11133=CARTESIAN_POINT('Ctrl Pts',(1.1,-1.26098326598685,0.700000000000001));
#11134=CARTESIAN_POINT('Ctrl Pts',(1.1,-1.25565664448621,0.7));
#11135=CARTESIAN_POINT('',(1.1,-1.39262953588351,0.));
#11136=CARTESIAN_POINT('Ctrl Pts',(1.1,-1.39262953588351,0.));
#11137=CARTESIAN_POINT('Ctrl Pts',(1.1,-1.38665944902278,0.100890429980357));
#11138=CARTESIAN_POINT('Ctrl Pts',(1.1,-1.38068638286488,0.201781712214768));
#11139=CARTESIAN_POINT('Ctrl Pts',(1.1,-1.36872453529477,0.403729561179669));
#11140=CARTESIAN_POINT('Ctrl Pts',(1.10000000000005,-1.3627356212621,0.504788200493074));
#11141=CARTESIAN_POINT('Ctrl Pts',(1.10000000000005,-1.35674377243284,0.605845626926786));
#11142=CARTESIAN_POINT('',(1.1,-1.44962962962963,0.));
#11143=CARTESIAN_POINT('Origin',(0.199725906950915,-1.4,-0.0104671912485888));
#11144=CARTESIAN_POINT('',(0.200274469199584,1.15262458915154,1.38777878078145E-17));
#11145=CARTESIAN_POINT('',(0.200274469199585,-0.7,0.));
#11146=CARTESIAN_POINT('',(0.231993417893744,1.12115139781563,0.605233595624295));
#11147=CARTESIAN_POINT('Ctrl Pts',(0.200274469199584,1.15262458915154,-5.50774703622636E-17));
#11148=CARTESIAN_POINT('Ctrl Pts',(0.210847451072758,1.1421331482829,0.201744512318911));
#11149=CARTESIAN_POINT('Ctrl Pts',(0.221420433966108,1.13164208276446,0.403489044103923));
#11150=CARTESIAN_POINT('Ctrl Pts',(0.231993417893744,1.12115139781563,0.605233595624295));
#11151=CARTESIAN_POINT('',(0.231993417893744,-1.12115139781563,0.605233595624295));
#11152=CARTESIAN_POINT('',(0.231993417893744,-0.7,0.605233595624295));
#11153=CARTESIAN_POINT('',(0.200274469199584,-1.15262458915154,1.38777878078145E-17));
#11154=CARTESIAN_POINT('Ctrl Pts',(0.231993417893744,-1.12115139781563,
0.605233595624295));
#11155=CARTESIAN_POINT('Ctrl Pts',(0.221420433966108,-1.13164208276446,
0.403489044103923));
#11156=CARTESIAN_POINT('Ctrl Pts',(0.210847451072758,-1.1421331482829,0.201744512318911));
#11157=CARTESIAN_POINT('Ctrl Pts',(0.200274469199584,-1.15262458915154,
-6.67868538251071E-17));
#11158=CARTESIAN_POINT('',(0.200274469199585,-0.7,0.));
#11159=CARTESIAN_POINT('Origin',(6.07974599480623,0.,0.));
#11160=CARTESIAN_POINT('Ctrl Pts',(8.1,-1.69866351109718,4.37041895728907E-16));
#11161=CARTESIAN_POINT('Ctrl Pts',(8.9524267631348,-1.65897367198627,1.20944032620455E-7));
#11162=CARTESIAN_POINT('Ctrl Pts',(9.80407798130771,-1.59837060538327,2.76830114922109E-8));
#11163=CARTESIAN_POINT('Ctrl Pts',(10.6537697771985,-1.52488560579501,1.03413542584124E-8));
#11164=CARTESIAN_POINT('Ctrl Pts',(10.8359404901627,-1.50913069933138,6.62336842220622E-9));
#11165=CARTESIAN_POINT('Ctrl Pts',(11.0180211259896,-1.49278349820154,3.93228299510406E-9));
#11166=CARTESIAN_POINT('Ctrl Pts',(11.2000000002909,-1.47592264092474,-3.0227174540096E-11));
#11167=CARTESIAN_POINT('Ctrl Pts',(11.2000000002909,1.47592264092474,-3.02272213335841E-11));
#11168=CARTESIAN_POINT('Ctrl Pts',(10.4240589919717,1.54781576943643,1.68591524001238E-8));
#11169=CARTESIAN_POINT('Ctrl Pts',(9.64626799696257,1.61037563220813,6.17878738288937E-8));
#11170=CARTESIAN_POINT('Ctrl Pts',(8.86753211358286,1.65747704847969,5.27022751808308E-8));
#11171=CARTESIAN_POINT('Ctrl Pts',(8.61177933690776,1.67294611604661,4.97183789310355E-8));
#11172=CARTESIAN_POINT('Ctrl Pts',(8.35592462822135,1.68674740550612,3.63007687033005E-8));
#11173=CARTESIAN_POINT('Ctrl Pts',(8.1,1.69866351109718,3.71000138306103E-16));
#11174=CARTESIAN_POINT('',(7.9,1.70758761671949,0.));
#11175=CARTESIAN_POINT('',(7.9,1.7737037037037,0.));
#11176=CARTESIAN_POINT('Ctrl Pts',(7.90000000036908,1.70758761645525,-3.06814577203155E-11));
#11177=CARTESIAN_POINT('Ctrl Pts',(7.26247716501442,1.73478515342832,3.65175246633048E-8));
#11178=CARTESIAN_POINT('Ctrl Pts',(6.624575449312,1.74993328406844,-3.04558542439636E-7));
#11179=CARTESIAN_POINT('Ctrl Pts',(5.98677261990733,1.74972113442148,-3.1918790057331E-7));
#11180=CARTESIAN_POINT('Ctrl Pts',(5.35540610719671,1.74951112565922,-3.33669628155763E-7));
#11181=CARTESIAN_POINT('Ctrl Pts',(4.72663057529054,1.73425216511322,1.21151810208783E-7));
#11182=CARTESIAN_POINT('Ctrl Pts',(4.10000000045307,1.7011388979176,-4.27317258673188E-11));
#11183=CARTESIAN_POINT('',(3.9,1.68995649764597,0.));
#11184=CARTESIAN_POINT('',(3.9,1.7662962962963,0.));
#11185=CARTESIAN_POINT('Ctrl Pts',(3.9,1.68995649764597,-1.6113354923472E-17));
#11186=CARTESIAN_POINT('Ctrl Pts',(2.96252047830716,1.63464572816558,-1.61179993858831E-17));
#11187=CARTESIAN_POINT('Ctrl Pts',(2.02971500398675,1.53866944530133,-1.61823222708931E-17));
#11188=CARTESIAN_POINT('Ctrl Pts',(1.1,1.39262953588351,-1.60717230190728E-17));
#11189=CARTESIAN_POINT('',(0.9,1.3604297237941,0.));
#11190=CARTESIAN_POINT('',(0.9,1.44962962962963,0.));
#11191=CARTESIAN_POINT('',(0.28146619846596,1.25073018526678,0.));
#11192=CARTESIAN_POINT('Ctrl Pts',(0.899999999999963,1.36042972379409,2.53412200078296E-14));
#11193=CARTESIAN_POINT('Ctrl Pts',(0.693681964344164,1.32640030945436,-1.68820282978727E-7));
#11194=CARTESIAN_POINT('Ctrl Pts',(0.487510176034459,1.28986876146525,1.95094241611213E-11));
#11195=CARTESIAN_POINT('Ctrl Pts',(0.281466198465954,1.25073018526678,9.09211941846344E-16));
#11196=CARTESIAN_POINT('Ctrl Pts',(0.28146619846596,1.25073018526678,4.90059381963448E-17));
#11197=CARTESIAN_POINT('Ctrl Pts',(0.273672142824666,1.24924968434803,-1.60851827685828E-11));
#11198=CARTESIAN_POINT('Ctrl Pts',(0.266112037439191,1.2468180315926,-2.29735811958388E-6));
#11199=CARTESIAN_POINT('Ctrl Pts',(0.258922416881026,1.24354471831116,-3.39045428380668E-6));
#11200=CARTESIAN_POINT('Ctrl Pts',(0.254316658841251,1.24144779416325,-4.09070493067818E-6));
#11201=CARTESIAN_POINT('Ctrl Pts',(0.249862973385875,1.23900427835211,-4.3601744978078E-6));
#11202=CARTESIAN_POINT('Ctrl Pts',(0.245601965247185,1.23623285256398,-4.0505643599354E-6));
#11203=CARTESIAN_POINT('Ctrl Pts',(0.238945660500109,1.23190348870705,-3.5669089987193E-6));
#11204=CARTESIAN_POINT('Ctrl Pts',(0.232836306411817,1.22682685988243,-1.47564048465526E-6));
#11205=CARTESIAN_POINT('Ctrl Pts',(0.227416445112993,1.2210931256102,-3.43092614100725E-7));
#11206=CARTESIAN_POINT('Ctrl Pts',(0.225957664245637,1.21954986437275,-3.82620891408318E-8));
#11207=CARTESIAN_POINT('Ctrl Pts',(0.224549002474426,1.21795876469157,1.76022586487844E-7));
#11208=CARTESIAN_POINT('Ctrl Pts',(0.223193686986583,1.21632111005909,2.01577349231486E-7));
#11209=CARTESIAN_POINT('Ctrl Pts',(0.221344954485829,1.21408724984631,2.36435595047204E-7));
#11210=CARTESIAN_POINT('Ctrl Pts',(0.219595448227346,1.21176677459781,-7.7718209010198E-8));
#11211=CARTESIAN_POINT('Ctrl Pts',(0.217948412504407,1.20936721934621,-5.08402878561E-7));
#11212=CARTESIAN_POINT('Ctrl Pts',(0.213467776427723,1.20283941082417,-1.68004793834142E-6));
#11213=CARTESIAN_POINT('Ctrl Pts',(0.20978887558685,1.19579640990262,-3.43350901357988E-6));
#11214=CARTESIAN_POINT('Ctrl Pts',(0.206958221875648,1.18840352636746,-3.67425174897535E-6));
#11215=CARTESIAN_POINT('Ctrl Pts',(0.206193447398199,1.18640614723908,-3.7392946395744E-6));
#11216=CARTESIAN_POINT('Ctrl Pts',(0.205490847532167,1.18438308363371,-3.7149036306613E-6));
#11217=CARTESIAN_POINT('Ctrl Pts',(0.204851940804359,1.18233735619935,-3.6037364623937E-6));
#11218=CARTESIAN_POINT('Ctrl Pts',(0.202492508448082,1.17478264548698,-3.19320484275276E-6));
#11219=CARTESIAN_POINT('Ctrl Pts',(0.201019195184615,1.16698811697394,-1.36638523817118E-6));
#11220=CARTESIAN_POINT('Ctrl Pts',(0.200491965466086,1.15911075533121,-4.28455138775697E-7));
#11221=CARTESIAN_POINT('Ctrl Pts',(0.200347608840846,1.15695391685535,-1.71647870329038E-7));
#11222=CARTESIAN_POINT('Ctrl Pts',(0.200274469313241,1.15479080601565,-7.49035961899928E-12));
#11223=CARTESIAN_POINT('Ctrl Pts',(0.200274469199584,1.15262458915154,9.10729824887824E-18));
#11224=CARTESIAN_POINT('',(2.01407162049393E-18,1.15316892111334,2.77409355997279E-17));
#11225=CARTESIAN_POINT('',(0.,-1.4,0.));
#11226=CARTESIAN_POINT('',(0.243580684154574,1.44748675362873,2.77555756156289E-17));
#11227=CARTESIAN_POINT('Ctrl Pts',(0.243580684154575,1.44748675362873,-1.56125112837913E-16));
#11228=CARTESIAN_POINT('Ctrl Pts',(0.226022619058538,1.44415189332774,-6.74769223000006E-12));
#11229=CARTESIAN_POINT('Ctrl Pts',(0.208837776424359,1.43922483814223,-1.83343972289099E-6));
#11230=CARTESIAN_POINT('Ctrl Pts',(0.192216855517481,1.43283671850359,-2.37047811876899E-6));
#11231=CARTESIAN_POINT('Ctrl Pts',(0.175448307189507,1.42639185943196,-2.91228650265529E-6));
#11232=CARTESIAN_POINT('Ctrl Pts',(0.15925228528901,1.41845922211561,-2.09168970691363E-6));
#11233=CARTESIAN_POINT('Ctrl Pts',(0.143842215871583,1.4091253227419,-1.20497646612983E-7));
#11234=CARTESIAN_POINT('Ctrl Pts',(0.141154971457358,1.40749765525544,2.23243494969264E-7));
#11235=CARTESIAN_POINT('Ctrl Pts',(0.138491701959641,1.40582727297256,5.92673833856784E-7));
#11236=CARTESIAN_POINT('Ctrl Pts',(0.135853645420207,1.40411450883245,9.74556207071009E-7));
#11237=CARTESIAN_POINT('Ctrl Pts',(0.120686164410185,1.39426698768136,3.17018528370531E-6));
#11238=CARTESIAN_POINT('Ctrl Pts',(0.106484701177391,1.38310949089167,6.09567884445769E-6));
#11239=CARTESIAN_POINT('Ctrl Pts',(0.0934509959242968,1.37075049507673,
5.10227143121889E-6));
#11240=CARTESIAN_POINT('Ctrl Pts',(0.0918301157095608,1.36921352217444,
4.97873062758527E-6));
#11241=CARTESIAN_POINT('Ctrl Pts',(0.0902273306836925,1.36765791150105,
4.78983320752683E-6));
#11242=CARTESIAN_POINT('Ctrl Pts',(0.0886430622088043,1.36608382581751,
4.52250464763623E-6));
#11243=CARTESIAN_POINT('Ctrl Pts',(0.0755027622673366,1.35302798437193,
2.30521792157715E-6));
#11244=CARTESIAN_POINT('Ctrl Pts',(0.0636322991078783,1.33870385142449,
-4.95851449924696E-6));
#11245=CARTESIAN_POINT('Ctrl Pts',(0.0531272107863483,1.3233265665666,-1.07771754856876E-5));
#11246=CARTESIAN_POINT('Ctrl Pts',(0.0429100363670196,1.3083707283404,-1.64363639061758E-5));
#11247=CARTESIAN_POINT('Ctrl Pts',(0.0340657397255946,1.29253754778979,
-2.07072841115287E-5));
#11248=CARTESIAN_POINT('Ctrl Pts',(0.026663056477648,1.27603964904139,-2.15377272154938E-5));
#11249=CARTESIAN_POINT('Ctrl Pts',(0.0217318501145713,1.26504977678014,
-2.20909166714363E-5));
#11250=CARTESIAN_POINT('Ctrl Pts',(0.0174411483101006,1.25376411673155,
-2.12025196266096E-5));
#11251=CARTESIAN_POINT('Ctrl Pts',(0.01382286588119,1.24224013948332,-1.91534441809703E-5));
#11252=CARTESIAN_POINT('Ctrl Pts',(0.00842668188255806,1.22505366970124,
-1.60975223868617E-5));
#11253=CARTESIAN_POINT('Ctrl Pts',(0.00456091079961661,1.20745571355567,
-1.03588883906395E-5));
#11254=CARTESIAN_POINT('Ctrl Pts',(0.0023097402764219,1.18964331095195,
-5.71664032024866E-6));
#11255=CARTESIAN_POINT('Ctrl Pts',(0.00078319128522165,1.17756448131848,
-2.56866950429304E-6));
#11256=CARTESIAN_POINT('Ctrl Pts',(2.50028438421117E-9,1.16538650529032,
-1.91718613723104E-10));
#11257=CARTESIAN_POINT('Ctrl Pts',(-1.21430643318376E-17,1.15316892111333,
5.20417042793042E-18));
#11258=CARTESIAN_POINT('',(11.7295909468525,1.62672708026858,5.55111512312578E-17));
#11259=CARTESIAN_POINT('Ctrl Pts',(0.243580684154574,1.44748675362873,0.));
#11260=CARTESIAN_POINT('Ctrl Pts',(4.07225077172054,2.17467835246083,0.));
#11261=CARTESIAN_POINT('Ctrl Pts',(7.90092085928651,2.00057770191527,0.));
#11262=CARTESIAN_POINT('Ctrl Pts',(11.7295909468525,1.62672708026858,0.));
#11263=CARTESIAN_POINT('',(12.,1.32855945177638,-4.17473993839455E-17));
#11264=CARTESIAN_POINT('Ctrl Pts',(12.,1.32855945177638,2.42861286636753E-16));
#11265=CARTESIAN_POINT('Ctrl Pts',(11.9999999991614,1.34640852075174,-1.28298622986823E-11));
#11266=CARTESIAN_POINT('Ctrl Pts',(11.9983618543561,1.36418409382152,-2.22383001277967E-6));
#11267=CARTESIAN_POINT('Ctrl Pts',(11.9951861391139,1.38167870884165,-3.43465861540838E-6));
#11268=CARTESIAN_POINT('Ctrl Pts',(11.9919727904737,1.39938064150867,-4.65983598400874E-6));
#11269=CARTESIAN_POINT('Ctrl Pts',(11.9871848331028,1.41679645887758,-4.78742071954366E-6));
#11270=CARTESIAN_POINT('Ctrl Pts',(11.9808755917115,1.43370272794343,-3.5739118077222E-6));
#11271=CARTESIAN_POINT('Ctrl Pts',(11.9797611226834,1.43668906371449,-3.35955670324834E-6));
#11272=CARTESIAN_POINT('Ctrl Pts',(11.9785990681726,1.43965944485564,-3.11247275469786E-6));
#11273=CARTESIAN_POINT('Ctrl Pts',(11.9773895732386,1.44261255525912,-2.84353511336506E-6));
#11274=CARTESIAN_POINT('Ctrl Pts',(11.9705369081732,1.45934406518776,-1.31980853313606E-6));
#11275=CARTESIAN_POINT('Ctrl Pts',(11.9622259501015,1.47537448669426,1.24030492427686E-6));
#11276=CARTESIAN_POINT('Ctrl Pts',(11.9525330320198,1.49048867890869,8.79804099270529E-7));
#11277=CARTESIAN_POINT('Ctrl Pts',(11.9492586078121,1.49559449703792,7.58021100761347E-7));
#11278=CARTESIAN_POINT('Ctrl Pts',(11.9458260650319,1.50059560584699,2.73671093112169E-7));
#11279=CARTESIAN_POINT('Ctrl Pts',(11.9422371454499,1.50548309160802,-8.21070286398525E-7));
#11280=CARTESIAN_POINT('Ctrl Pts',(11.9335276940755,1.51734385321214,-3.47774636801117E-6));
#11281=CARTESIAN_POINT('Ctrl Pts',(11.923898315087,1.52853671512454,-9.61160164537397E-6));
#11282=CARTESIAN_POINT('Ctrl Pts',(11.9134480753511,1.53899918600446,-1.54908303532852E-5));
#11283=CARTESIAN_POINT('Ctrl Pts',(11.9006414429521,1.55182080751067,-2.26957483986032E-5));
#11284=CARTESIAN_POINT('Ctrl Pts',(11.8867118754531,1.56343792791748,-2.93307907620841E-5));
#11285=CARTESIAN_POINT('Ctrl Pts',(11.8718669715436,1.57375979462261,-3.2097080434168E-5));
#11286=CARTESIAN_POINT('Ctrl Pts',(11.8583226919989,1.58317731924447,-3.46210038525051E-5));
#11287=CARTESIAN_POINT('Ctrl Pts',(11.84401509256,1.59151672629289,-3.39892197405707E-5));
#11288=CARTESIAN_POINT('Ctrl Pts',(11.8290799708805,1.59867837245092,-3.04453078860132E-5));
#11289=CARTESIAN_POINT('Ctrl Pts',(11.8128282236205,1.60647136308226,-2.65889777530425E-5));
#11290=CARTESIAN_POINT('Ctrl Pts',(11.7959622791259,1.61280865470064,-1.93051308245346E-5));
#11291=CARTESIAN_POINT('Ctrl Pts',(11.7786680578171,1.61758555622507,-1.24065785496921E-5));
#11292=CARTESIAN_POINT('Ctrl Pts',(11.7626326571209,1.62201475420184,-6.0101616208217E-6));
#11293=CARTESIAN_POINT('Ctrl Pts',(11.7462278952123,1.62510256303752,-1.15598952599692E-10));
#11294=CARTESIAN_POINT('Ctrl Pts',(11.7295909468525,1.62672708026857,-1.01481323344643E-16));
#11295=CARTESIAN_POINT('',(12.,-1.32855945177638,-2.7831599589297E-17));
#11296=CARTESIAN_POINT('',(12.,1.6,0.));
#11297=CARTESIAN_POINT('',(11.7295909468525,-1.62672708026858,-2.77555756156289E-17));
#11298=CARTESIAN_POINT('Ctrl Pts',(11.7295909468525,-1.62672708026858,2.76688394418301E-16));
#11299=CARTESIAN_POINT('Ctrl Pts',(11.7473502233519,-1.62499297457843,3.63491969896433E-13));
#11300=CARTESIAN_POINT('Ctrl Pts',(11.7648769397846,-1.62163540491215,-2.46542030701863E-6));
#11301=CARTESIAN_POINT('Ctrl Pts',(11.7819744899096,-1.61677476461769,-3.87870576098494E-6));
#11302=CARTESIAN_POINT('Ctrl Pts',(11.799277951102,-1.61185558613358,-5.30901184740094E-6));
#11303=CARTESIAN_POINT('Ctrl Pts',(11.8161433440738,-1.60539638769883,-5.61072687595782E-6));
#11304=CARTESIAN_POINT('Ctrl Pts',(11.8323535184498,-1.59747214364331,-4.43708131311936E-6));
#11305=CARTESIAN_POINT('Ctrl Pts',(11.8351986841263,-1.59608130189932,-4.23108623901291E-6));
#11306=CARTESIAN_POINT('Ctrl Pts',(11.8380235988884,-1.59464521634493,-3.98890160078043E-6));
#11307=CARTESIAN_POINT('Ctrl Pts',(11.8408269920241,-1.59316415515964,-3.72087260345577E-6));
#11308=CARTESIAN_POINT('Ctrl Pts',(11.8568148563263,-1.58471760338924,-2.19229240409177E-6));
#11309=CARTESIAN_POINT('Ctrl Pts',(11.8719627312575,-1.57488689795395,5.08047814114288E-7));
#11310=CARTESIAN_POINT('Ctrl Pts',(11.8860639991294,-1.56376935451958,3.7910357452838E-7));
#11311=CARTESIAN_POINT('Ctrl Pts',(11.8908390360804,-1.5600046802233,3.35439876042474E-7));
#11312=CARTESIAN_POINT('Ctrl Pts',(11.8954938739134,-1.55609205312677,-6.31409548673105E-8));
#11313=CARTESIAN_POINT('Ctrl Pts',(11.9000197537765,-1.55203410647271,-1.07033715310124E-6));
#11314=CARTESIAN_POINT('Ctrl Pts',(11.9109521284419,-1.54223203603875,-3.50324446252274E-6));
#11315=CARTESIAN_POINT('Ctrl Pts',(11.9211333865357,-1.53158293117673,-9.37257606292525E-6));
#11316=CARTESIAN_POINT('Ctrl Pts',(11.9305114837192,-1.52019095639426,-1.50133174764804E-5));
#11317=CARTESIAN_POINT('Ctrl Pts',(11.9420285825687,-1.50620064502377,-2.19406264148308E-5));
#11318=CARTESIAN_POINT('Ctrl Pts',(11.9522379825693,-1.49120969914507,-2.8349487615449E-5));
#11319=CARTESIAN_POINT('Ctrl Pts',(11.9610699533786,-1.47543375940277,-3.10096306454085E-5));
#11320=CARTESIAN_POINT('Ctrl Pts',(11.9691383866925,-1.46102167397773,-3.34398002084833E-5));
#11321=CARTESIAN_POINT('Ctrl Pts',(11.976057247492,-1.44595309822982,-3.28127654573608E-5));
#11322=CARTESIAN_POINT('Ctrl Pts',(11.9817405815488,-1.43037347552767,-2.93737351251587E-5));
#11323=CARTESIAN_POINT('Ctrl Pts',(11.9879190063177,-1.41343666945002,-2.56351214921306E-5));
#11324=CARTESIAN_POINT('Ctrl Pts',(11.9925890154887,-1.39602986621001,-1.86015881889918E-5));
#11325=CARTESIAN_POINT('Ctrl Pts',(11.9956646601292,-1.37834843064327,-1.1951505214167E-5));
#11326=CARTESIAN_POINT('Ctrl Pts',(11.9985188379205,-1.36194017591583,-5.78027239782095E-6));
#11327=CARTESIAN_POINT('Ctrl Pts',(11.9999999979315,-1.34529424449622,-1.63143103698095E-10));
#11328=CARTESIAN_POINT('Ctrl Pts',(12.,-1.32855945177638,6.07153216591882E-17));
#11329=CARTESIAN_POINT('',(0.243580684154574,-1.44748675362873,-2.77555756156289E-17));
#11330=CARTESIAN_POINT('Ctrl Pts',(11.7295909468525,-1.62672708026858,0.));
#11331=CARTESIAN_POINT('Ctrl Pts',(7.90092085928651,-2.00057770191527,0.));
#11332=CARTESIAN_POINT('Ctrl Pts',(4.07225077172054,-2.17467835246083,0.));
#11333=CARTESIAN_POINT('Ctrl Pts',(0.243580684154574,-1.44748675362873,
0.));
#11334=CARTESIAN_POINT('',(-2.01407162049393E-18,-1.15316892111334,-2.77409355997279E-17));
#11335=CARTESIAN_POINT('Ctrl Pts',(-1.45716771982052E-16,-1.15316892111333,
-8.67361737988404E-17));
#11336=CARTESIAN_POINT('Ctrl Pts',(1.25998894435939E-9,-1.17105087373522,
-1.90287520688926E-11));
#11337=CARTESIAN_POINT('Ctrl Pts',(0.00163339464743996,-1.18886359576077,
-1.42965894531121E-6));
#11338=CARTESIAN_POINT('Ctrl Pts',(0.00480727841906161,-1.20639511031145,
-1.64093682142839E-6));
#11339=CARTESIAN_POINT('Ctrl Pts',(0.00800796397580062,-1.22407466931478,
-1.8539988284852E-6));
#11340=CARTESIAN_POINT('Ctrl Pts',(0.0127756311263789,-1.24146980201313,
-7.66483898132055E-7));
#11341=CARTESIAN_POINT('Ctrl Pts',(0.0190655400899108,-1.25835467436912,
1.24978183846727E-6));
#11342=CARTESIAN_POINT('Ctrl Pts',(0.0201762582672253,-1.26133632875492,
1.60582880463507E-6));
#11343=CARTESIAN_POINT('Ctrl Pts',(0.0213345630164365,-1.2643020159517,
1.98173645466097E-6));
#11344=CARTESIAN_POINT('Ctrl Pts',(0.022540357064946,-1.26725040777374,
2.36324320385681E-6));
#11345=CARTESIAN_POINT('Ctrl Pts',(0.0293845669280623,-1.28398578013164,
4.5287143794027E-6));
#11346=CARTESIAN_POINT('Ctrl Pts',(0.0376942987862453,-1.30001720705818,
7.20349268724091E-6));
#11347=CARTESIAN_POINT('Ctrl Pts',(0.0474014865253391,-1.31512615530125,
5.82569015349308E-6));
#11348=CARTESIAN_POINT('Ctrl Pts',(0.0485928463173857,-1.31698047129067,
5.65659292531477E-6));
#11349=CARTESIAN_POINT('Ctrl Pts',(0.049805315173965,-1.3188208685659,5.4220814195758E-6));
#11350=CARTESIAN_POINT('Ctrl Pts',(0.0510388164126442,-1.32064691964073,
5.10992468070797E-6));
#11351=CARTESIAN_POINT('Ctrl Pts',(0.0614399911345998,-1.33604461498541,
2.47774509321499E-6));
#11352=CARTESIAN_POINT('Ctrl Pts',(0.0733332132114129,-1.35042574344132,
-5.3152380038924E-6));
#11353=CARTESIAN_POINT('Ctrl Pts',(0.0865238753361435,-1.36365441213776,
-1.1550981620978E-5));
#11354=CARTESIAN_POINT('Ctrl Pts',(0.0993129767592984,-1.37648036310613,
-1.75968917362996E-5));
#11355=CARTESIAN_POINT('Ctrl Pts',(0.113220041589059,-1.38812080263946,
-2.21381304374214E-5));
#11356=CARTESIAN_POINT('Ctrl Pts',(0.128049501721596,-1.3984678073416,-2.30260298918279E-5));
#11357=CARTESIAN_POINT('Ctrl Pts',(0.137898881094142,-1.40534004502052,
-2.36157518704412E-5));
#11358=CARTESIAN_POINT('Ctrl Pts',(0.148156110210342,-1.41164106947418,
-2.26770903305374E-5));
#11359=CARTESIAN_POINT('Ctrl Pts',(0.158771208267938,-1.41732893485082,
-2.05010084084185E-5));
#11360=CARTESIAN_POINT('Ctrl Pts',(0.174640735071984,-1.42583226958806,
-1.72477751171679E-5));
#11361=CARTESIAN_POINT('Ctrl Pts',(0.191199787345415,-1.4329086754137,-1.11085100333009E-5));
#11362=CARTESIAN_POINT('Ctrl Pts',(0.208270835533445,-1.43843835369108,
-6.12965879291162E-6));
#11363=CARTESIAN_POINT('Ctrl Pts',(0.219822542278978,-1.44218019901621,
-2.76054936125183E-6));
#11364=CARTESIAN_POINT('Ctrl Pts',(0.231609382520684,-1.4452130041726,-1.10646384277296E-10));
#11365=CARTESIAN_POINT('Ctrl Pts',(0.243580684154575,-1.44748675362873,
-8.67361737988404E-18));
#11366=CARTESIAN_POINT('',(0.,-1.4,0.));
#11367=CARTESIAN_POINT('',(0.28146619846596,-1.25073018526678,-1.38777878078145E-17));
#11368=CARTESIAN_POINT('Ctrl Pts',(0.200274469199584,-1.15262458915154,
-4.38017677684144E-17));
#11369=CARTESIAN_POINT('Ctrl Pts',(0.200274469606231,-1.16056122076396,
-2.67994619525583E-11));
#11370=CARTESIAN_POINT('Ctrl Pts',(0.201251993787099,-1.16844573575355,
-2.06906772440415E-6));
#11371=CARTESIAN_POINT('Ctrl Pts',(0.203125250303271,-1.17612349127761,
-3.03593176598444E-6));
#11372=CARTESIAN_POINT('Ctrl Pts',(0.204328175564463,-1.18105381768481,
-3.65681052429326E-6));
#11373=CARTESIAN_POINT('Ctrl Pts',(0.205901645655995,-1.18589907428975,
-3.87486521964464E-6));
#11374=CARTESIAN_POINT('Ctrl Pts',(0.207834893326199,-1.19061551412018,
-3.56660141708203E-6));
#11375=CARTESIAN_POINT('Ctrl Pts',(0.210845733886816,-1.19796089907112,
-3.08651126907409E-6));
#11376=CARTESIAN_POINT('Ctrl Pts',(0.214691665920849,-1.20490884791767,
-1.13290501265697E-6));
#11377=CARTESIAN_POINT('Ctrl Pts',(0.219311372289421,-1.21130241743461,
-1.88024479619773E-7));
#11378=CARTESIAN_POINT('Ctrl Pts',(0.220549822002528,-1.21301640393121,
6.52788543367939E-8));
#11379=CARTESIAN_POINT('Ctrl Pts',(0.22184414018537,-1.21469042595737,2.26073670777299E-7));
#11380=CARTESIAN_POINT('Ctrl Pts',(0.223193686901845,-1.21632111014354,
1.99977909429435E-7));
#11381=CARTESIAN_POINT('Ctrl Pts',(0.225054776233359,-1.21856990146355,
1.63990609064731E-7));
#11382=CARTESIAN_POINT('Ctrl Pts',(0.227020882846909,-1.2207363067163,-2.2494482424301E-7));
#11383=CARTESIAN_POINT('Ctrl Pts',(0.229085096241527,-1.22281561536867,
-7.25033596408456E-7));
#11384=CARTESIAN_POINT('Ctrl Pts',(0.234663732853057,-1.22843504764494,
-2.07654770860772E-6));
#11385=CARTESIAN_POINT('Ctrl Pts',(0.240898147116973,-1.23336261820331,
-3.93931381885212E-6));
#11386=CARTESIAN_POINT('Ctrl Pts',(0.247634917667946,-1.2375211924479,-4.15647360184107E-6));
#11387=CARTESIAN_POINT('Ctrl Pts',(0.24944409362824,-1.23863798757926,-4.21479238469909E-6));
#11388=CARTESIAN_POINT('Ctrl Pts',(0.251289686356224,-1.23969909864123,
-4.17584617698396E-6));
#11389=CARTESIAN_POINT('Ctrl Pts',(0.253169062337335,-1.24070249413235,
-4.04352721072409E-6));
#11390=CARTESIAN_POINT('Ctrl Pts',(0.260147540238377,-1.24442829106235,
-3.55220190316667E-6));
#11391=CARTESIAN_POINT('Ctrl Pts',(0.267526846148503,-1.24732811138375,
-1.51439637010182E-6));
#11392=CARTESIAN_POINT('Ctrl Pts',(0.275164162321015,-1.24931347733136,
-4.73394739174148E-7));
#11393=CARTESIAN_POINT('Ctrl Pts',(0.277246452424842,-1.24985478107889,
-1.89568936341825E-7));
#11394=CARTESIAN_POINT('Ctrl Pts',(0.27934803608603,-1.25032783487679,-4.20368826828312E-12));
#11395=CARTESIAN_POINT('Ctrl Pts',(0.28146619846596,-1.25073018526678,1.2793585635329E-17));
#11396=CARTESIAN_POINT('',(0.9,-1.3604297237941,0.));
#11397=CARTESIAN_POINT('Ctrl Pts',(0.281466198465954,-1.25073018526678,
9.63150999927498E-16));
#11398=CARTESIAN_POINT('Ctrl Pts',(0.487510152792939,-1.28986875705046,
1.95065110193295E-11));
#11399=CARTESIAN_POINT('Ctrl Pts',(0.693681940810289,-1.32640030557063,
-1.68784634270162E-7));
#11400=CARTESIAN_POINT('Ctrl Pts',(0.899999999999961,-1.36042972379409,
2.52314774976951E-14));
#11401=CARTESIAN_POINT('',(0.9,1.44962962962963,0.));
#11402=CARTESIAN_POINT('',(3.9,-1.68995649764597,0.));
#11403=CARTESIAN_POINT('Ctrl Pts',(1.1,-1.39262953588351,-2.05019623674552E-17));
#11404=CARTESIAN_POINT('Ctrl Pts',(2.02971449277185,-1.53866936499954,-2.04062575199768E-17));
#11405=CARTESIAN_POINT('Ctrl Pts',(2.96251993741879,-1.63464569625347,-2.05230086706555E-17));
#11406=CARTESIAN_POINT('Ctrl Pts',(3.9,-1.68995649764597,-2.05203881127908E-17));
#11407=CARTESIAN_POINT('',(3.9,1.7662962962963,0.));
#11408=CARTESIAN_POINT('',(7.9,-1.70758761671949,0.));
#11409=CARTESIAN_POINT('Ctrl Pts',(4.10000000045307,-1.7011388979176,-4.27317380631109E-11));
#11410=CARTESIAN_POINT('Ctrl Pts',(4.72643887491804,-1.7342420350347,1.20853286712337E-7));
#11411=CARTESIAN_POINT('Ctrl Pts',(5.35502164560988,-1.74950180199062,-3.33551248611792E-7));
#11412=CARTESIAN_POINT('Ctrl Pts',(5.98619394951577,-1.74972093772735,-3.1920111515717E-7));
#11413=CARTESIAN_POINT('Ctrl Pts',(6.62418968669829,-1.74994244248134,-3.0469584628258E-7));
#11414=CARTESIAN_POINT('Ctrl Pts',(7.26228442347589,-1.73479337602516,3.6583895104054E-8));
#11415=CARTESIAN_POINT('Ctrl Pts',(7.90000000036908,-1.70758761645525,-3.06816097140251E-11));
#11416=CARTESIAN_POINT('',(7.9,1.7737037037037,0.));
#11417=CARTESIAN_POINT('',(11.4,-1.45718524058191,0.));
#11418=CARTESIAN_POINT('',(11.7095901160181,-1.42740242188993,1.38777878078145E-17));
#11419=CARTESIAN_POINT('Ctrl Pts',(11.4000000008084,-1.45718524050535,1.02728155843002E-16));
#11420=CARTESIAN_POINT('Ctrl Pts',(11.5032315878449,-1.44740895658952,-1.62414911853346E-10));
#11421=CARTESIAN_POINT('Ctrl Pts',(11.6064290066394,-1.43747657129068,3.17212713797596E-13));
#11422=CARTESIAN_POINT('Ctrl Pts',(11.7095901160181,-1.42740242188993,-1.31135713082882E-16));
#11423=CARTESIAN_POINT('',(11.7997255308004,-1.32801330383774,0.));
#11424=CARTESIAN_POINT('Ctrl Pts',(11.7095901160181,-1.42740242188993,-9.19403442267708E-17));
#11425=CARTESIAN_POINT('Ctrl Pts',(11.7174875668098,-1.42663119997609,-1.06723531187443E-12));
#11426=CARTESIAN_POINT('Ctrl Pts',(11.7252481284326,-1.42489860698852,-1.31351091787008E-6));
#11427=CARTESIAN_POINT('Ctrl Pts',(11.7327147629935,-1.4222933789697,-1.57347087725304E-6));
#11428=CARTESIAN_POINT('Ctrl Pts',(11.7375034508718,-1.42062252930751,-1.7401948673154E-6));
#11429=CARTESIAN_POINT('Ctrl Pts',(11.742171336984,-1.41859157258352,-1.52962160850981E-6));
#11430=CARTESIAN_POINT('Ctrl Pts',(11.7466731630754,-1.4162133745499,-1.06822103866601E-6));
#11431=CARTESIAN_POINT('Ctrl Pts',(11.7538080604269,-1.41244419322064,-3.36952074275293E-7));
#11432=CARTESIAN_POINT('Ctrl Pts',(11.7604421378066,-1.40785009750528,1.23525126371337E-6));
#11433=CARTESIAN_POINT('Ctrl Pts',(11.7664060685299,-1.40250292630552,-7.85770423176645E-8));
#11434=CARTESIAN_POINT('Ctrl Pts',(11.7700505374369,-1.39923534992309,-8.81437879006801E-7));
#11435=CARTESIAN_POINT('Ctrl Pts',(11.7734443324447,-1.39568546479044,-2.84121358692309E-6));
#11436=CARTESIAN_POINT('Ctrl Pts',(11.7765701913309,-1.39188797822873,-4.73246891796253E-6));
#11437=CARTESIAN_POINT('Ctrl Pts',(11.7816218974528,-1.38575085342217,-7.78893003218221E-6));
#11438=CARTESIAN_POINT('Ctrl Pts',(11.7859196635778,-1.3790373064984,-1.04294718165207E-5));
#11439=CARTESIAN_POINT('Ctrl Pts',(11.7894058487846,-1.37190723377291,-1.0649753115785E-5));
#11440=CARTESIAN_POINT('Ctrl Pts',(11.7909886780302,-1.36866997385604,-1.07497672177443E-5));
#11441=CARTESIAN_POINT('Ctrl Pts',(11.7924036476919,-1.36534638272796,-1.04045251440782E-5));
#11442=CARTESIAN_POINT('Ctrl Pts',(11.7936422141268,-1.36194984358789,-9.67400732978531E-6));
#11443=CARTESIAN_POINT('Ctrl Pts',(11.7963517531347,-1.35451943450186,-8.0758964348484E-6));
#11444=CARTESIAN_POINT('Ctrl Pts',(11.7981920551596,-1.34681816044402,-4.45435127417515E-6));
#11445=CARTESIAN_POINT('Ctrl Pts',(11.7990923524223,-1.33899256731255,-1.99131993767782E-6));
#11446=CARTESIAN_POINT('Ctrl Pts',(11.7995108157868,-1.33535518645399,-8.46488755312323E-7));
#11447=CARTESIAN_POINT('Ctrl Pts',(11.7997255306472,-1.33169069466208,-1.20180646731727E-11));
#11448=CARTESIAN_POINT('Ctrl Pts',(11.7997255308004,-1.32801330383774,1.56125112837913E-17));
#11449=CARTESIAN_POINT('',(11.7997255308004,1.32801330383774,-1.38777878078145E-17));
#11450=CARTESIAN_POINT('',(11.7997255308004,0.8,0.));
#11451=CARTESIAN_POINT('',(11.7095901160181,1.42740242188993,1.38777878078145E-17));
#11452=CARTESIAN_POINT('Ctrl Pts',(11.7997255308004,1.32801330383774,3.29597460435593E-17));
#11453=CARTESIAN_POINT('Ctrl Pts',(11.7997255306701,1.33594993357028,-3.19998942079111E-12));
#11454=CARTESIAN_POINT('Ctrl Pts',(11.7987557313351,1.34384388324515,-1.1738056914779E-6));
#11455=CARTESIAN_POINT('Ctrl Pts',(11.7968890528831,1.35153020534854,-1.35082478761126E-6));
#11456=CARTESIAN_POINT('Ctrl Pts',(11.7956902940742,1.35646627043222,-1.46450435604653E-6));
#11457=CARTESIAN_POINT('Ctrl Pts',(11.7941204989552,1.36131691981906,-1.21679535622301E-6));
#11458=CARTESIAN_POINT('Ctrl Pts',(11.7921880664813,1.36603565236267,-7.51718013047842E-7));
#11459=CARTESIAN_POINT('Ctrl Pts',(11.7891321441143,1.37349779167052,-1.62510435539431E-8));
#11460=CARTESIAN_POINT('Ctrl Pts',(11.7852081688769,1.38054242009704,1.47305143123643E-6));
#11461=CARTESIAN_POINT('Ctrl Pts',(11.7804707482717,1.38699431162271,4.31295153147674E-8));
#11462=CARTESIAN_POINT('Ctrl Pts',(11.7775673564694,1.39094843993989,-8.33217322910001E-7));
#11463=CARTESIAN_POINT('Ctrl Pts',(11.774357304366,1.39467961749964,-2.88177890715362E-6));
#11464=CARTESIAN_POINT('Ctrl Pts',(11.7708736118052,1.39816709864095,-4.85419454747415E-6));
#11465=CARTESIAN_POINT('Ctrl Pts',(11.7652557092992,1.40379111072049,-8.03496856102318E-6));
#11466=CARTESIAN_POINT('Ctrl Pts',(11.7589908599241,1.40872063947841,-1.07717451179728E-5));
#11467=CARTESIAN_POINT('Ctrl Pts',(11.7522324303862,1.41288246393566,-1.10093962897399E-5));
#11468=CARTESIAN_POINT('Ctrl Pts',(11.7491699691574,1.41476832010531,-1.11170836593312E-5));
#11469=CARTESIAN_POINT('Ctrl Pts',(11.7460056456443,1.41649603445901,-1.07652933077188E-5));
#11470=CARTESIAN_POINT('Ctrl Pts',(11.7427518690514,1.41805582819498,-1.00150721194158E-5));
#11471=CARTESIAN_POINT('Ctrl Pts',(11.7356218627913,1.421473806899,-8.37111113549047E-6));
#11472=CARTESIAN_POINT('Ctrl Pts',(11.7281378774234,1.42405291512428,-4.62166314666036E-6));
#11473=CARTESIAN_POINT('Ctrl Pts',(11.7204387731059,1.42570834923663,-2.06587013620581E-6));
#11474=CARTESIAN_POINT('Ctrl Pts',(11.7168648812537,1.42647679479109,-8.79481766934018E-7));
#11475=CARTESIAN_POINT('Ctrl Pts',(11.7132443218769,1.42704557200794,-8.45784208685192E-12));
#11476=CARTESIAN_POINT('Ctrl Pts',(11.7095901160181,1.42740242188993,2.53703308361608E-17));
#11477=CARTESIAN_POINT('',(11.4,1.45718524058191,0.));
#11478=CARTESIAN_POINT('Ctrl Pts',(11.7095901160181,1.42740242188993,-2.09644042577228E-16));
#11479=CARTESIAN_POINT('Ctrl Pts',(11.6064290073882,1.43747657121756,3.16925904777201E-13));
#11480=CARTESIAN_POINT('Ctrl Pts',(11.5032315885351,1.44740895652415,-1.62368751268212E-10));
#11481=CARTESIAN_POINT('Ctrl Pts',(11.4000000008083,1.45718524050537,-7.57963810214684E-17));
#11482=CARTESIAN_POINT('',(11.4,-1.53779953703704,0.));
#11483=CARTESIAN_POINT('Origin',(10.,0.,0.));
#11484=CARTESIAN_POINT('',(9.6,-4.89858719658942E-17,0.7));
#11485=CARTESIAN_POINT('Origin',(10.,0.,0.7));
#11486=CARTESIAN_POINT('',(9.6,-4.89858719658942E-17,0.));
#11487=CARTESIAN_POINT('Origin',(2.,0.,0.));
#11488=CARTESIAN_POINT('',(1.6,-4.89858719658941E-17,0.7));
#11489=CARTESIAN_POINT('Origin',(2.,0.,0.7));
#11490=CARTESIAN_POINT('',(1.6,-4.89858719658941E-17,0.));
#11491=CARTESIAN_POINT('Origin',(11.4,-1.53779953703704,0.));
#11492=CARTESIAN_POINT('',(11.4,-1.4227102204299,0.605660349289938));
#11493=CARTESIAN_POINT('Ctrl Pts',(11.4,-1.45718524058191,0.));
#11494=CARTESIAN_POINT('Ctrl Pts',(11.4,-1.45144762186897,0.100853500740053));
#11495=CARTESIAN_POINT('Ctrl Pts',(11.4,-1.44570843451869,0.201707502489292));
#11496=CARTESIAN_POINT('Ctrl Pts',(11.4,-1.43421679834229,0.403593890565801));
#11497=CARTESIAN_POINT('Ctrl Pts',(11.4,-1.42846427656079,0.504627461196798));
#11498=CARTESIAN_POINT('Ctrl Pts',(11.4,-1.4227102204299,0.605660349289938));
#11499=CARTESIAN_POINT('',(11.4,1.4227102204299,0.605660349289938));
#11500=CARTESIAN_POINT('Ctrl Pts',(11.4,1.4227102204299,0.605660349289938));
#11501=CARTESIAN_POINT('Ctrl Pts',(11.4,1.42846501637408,0.504614471147338));
#11502=CARTESIAN_POINT('Ctrl Pts',(11.4,1.43421827757761,0.403567910233218));
#11503=CARTESIAN_POINT('Ctrl Pts',(11.4,1.44570991295315,0.201681522149997));
#11504=CARTESIAN_POINT('Ctrl Pts',(11.4,1.45144836088146,0.100840510682596));
#11505=CARTESIAN_POINT('Ctrl Pts',(11.4,1.45718524058191,0.));
#11506=CARTESIAN_POINT('',(11.4,1.32241589772268,0.7));
#11507=CARTESIAN_POINT('Ctrl Pts',(11.3999999999682,1.32241589773435,0.7));
#11508=CARTESIAN_POINT('Ctrl Pts',(11.4000000023735,1.33035873561384,0.69999999792071));
#11509=CARTESIAN_POINT('Ctrl Pts',(11.3999980827719,1.33823923135401,0.699006238562837));
#11510=CARTESIAN_POINT('Ctrl Pts',(11.3999964146773,1.34591623266897,0.697118452648154));
#11511=CARTESIAN_POINT('Ctrl Pts',(11.3999954805754,1.35021521026861,0.696061327733467));
#11512=CARTESIAN_POINT('Ctrl Pts',(11.3999946303028,1.35445042327231,0.694722827332644));
#11513=CARTESIAN_POINT('Ctrl Pts',(11.3999940855437,1.35859537550353,0.6931136259882));
#11514=CARTESIAN_POINT('Ctrl Pts',(11.3999931076272,1.36603612757745,0.690224891070856));
#11515=CARTESIAN_POINT('Ctrl Pts',(11.3999932937992,1.3731074395729,0.686497549823264));
#11516=CARTESIAN_POINT('Ctrl Pts',(11.3999945206258,1.37966241828116,0.682010734965951));
#11517=CARTESIAN_POINT('Ctrl Pts',(11.3999951957832,1.38326980879772,0.679541513617388));
#11518=CARTESIAN_POINT('Ctrl Pts',(11.399996159718,1.38672054258633,0.67684140394947));
#11519=CARTESIAN_POINT('Ctrl Pts',(11.3999970106794,1.38998612808193,0.67391813047908));
#11520=CARTESIAN_POINT('Ctrl Pts',(11.399997834674,1.39314822810011,0.671087494715186));
#11521=CARTESIAN_POINT('Ctrl Pts',(11.3999985616145,1.39611771109305,0.668064564866167));
#11522=CARTESIAN_POINT('Ctrl Pts',(11.3999985600482,1.39887227052748,0.664860274403491));
#11523=CARTESIAN_POINT('Ctrl Pts',(11.3999985571253,1.40401282028653,0.65888043807832));
#11524=CARTESIAN_POINT('Ctrl Pts',(11.3999962993541,1.40840780441339,0.652270325570232));
#11525=CARTESIAN_POINT('Ctrl Pts',(11.399995545677,1.411994629421,0.6451936465425));
#11526=CARTESIAN_POINT('Ctrl Pts',(11.3999954685939,1.41236147527551,0.644469872631166));
#11527=CARTESIAN_POINT('Ctrl Pts',(11.3999954033687,1.41271982702329,0.643741199273148));
#11528=CARTESIAN_POINT('Ctrl Pts',(11.399995351278,1.41306958904162,0.643007791034547));
#11529=CARTESIAN_POINT('Ctrl Pts',(11.3999948427782,1.41648390439843,0.635848388696429));
#11530=CARTESIAN_POINT('Ctrl Pts',(11.3999960181446,1.41904356023948,0.628323447569199));
#11531=CARTESIAN_POINT('Ctrl Pts',(11.3999977140636,1.42069349507095,0.620600117586001));
#11532=CARTESIAN_POINT('Ctrl Pts',(11.3999987928026,1.4217429844709,0.615687467222433));
#11533=CARTESIAN_POINT('Ctrl Pts',(11.4,1.42242354791745,0.610693903223035));
#11534=CARTESIAN_POINT('Ctrl Pts',(11.4,1.42271022042989,0.605660349289938));
#11535=CARTESIAN_POINT('',(11.4,-1.32241589772233,0.7));
#11536=CARTESIAN_POINT('',(11.4,-0.768899768518519,0.7));
#11537=CARTESIAN_POINT('Ctrl Pts',(11.4,-1.4227102204299,0.605660349289938));
#11538=CARTESIAN_POINT('Ctrl Pts',(11.4,-1.42225988230954,0.613567634148305));
#11539=CARTESIAN_POINT('Ctrl Pts',(11.399997277834,-1.42084002197897,0.621378952482038));
#11540=CARTESIAN_POINT('Ctrl Pts',(11.3999960666067,-1.41853584574224,0.62893480307212));
#11541=CARTESIAN_POINT('Ctrl Pts',(11.3999954054252,-1.41727804822547,0.633059370437125));
#11542=CARTESIAN_POINT('Ctrl Pts',(11.399995101512,-1.41575577202439,0.637107840337094));
#11543=CARTESIAN_POINT('Ctrl Pts',(11.3999952458732,-1.4139766528271,0.641052464558972));
#11544=CARTESIAN_POINT('Ctrl Pts',(11.3999955106959,-1.41071295596475,0.648288661951321));
#11545=CARTESIAN_POINT('Ctrl Pts',(11.3999975070228,-1.40662392062869,0.655096264526915));
#11546=CARTESIAN_POINT('Ctrl Pts',(11.3999983091255,-1.40177626405188,0.661313589686923));
#11547=CARTESIAN_POINT('Ctrl Pts',(11.3999984645713,-1.40083679843637,0.66251849418371));
#11548=CARTESIAN_POINT('Ctrl Pts',(11.3999985618942,-1.3998687022723,0.663701157110503));
#11549=CARTESIAN_POINT('Ctrl Pts',(11.3999985615247,-1.39887227038638,0.664860274403572));
#11550=CARTESIAN_POINT('Ctrl Pts',(11.3999985608543,-1.39706426040285,0.666963474499402));
#11551=CARTESIAN_POINT('Ctrl Pts',(11.3999982409398,-1.39516298427334,0.668989190735049));
#11552=CARTESIAN_POINT('Ctrl Pts',(11.3999977953094,-1.39317470503404,0.670934323115149));
#11553=CARTESIAN_POINT('Ctrl Pts',(11.3999965209597,-1.38748891009577,0.67649673287249));
#11554=CARTESIAN_POINT('Ctrl Pts',(11.3999944455422,-1.38115857071774,0.681340422576046));
#11555=CARTESIAN_POINT('Ctrl Pts',(11.3999937508435,-1.37434881732181,0.685413525744465));
#11556=CARTESIAN_POINT('Ctrl Pts',(11.3999933041982,-1.36997059693002,0.688032261301096));
#11557=CARTESIAN_POINT('Ctrl Pts',(11.3999933336943,-1.3653932120823,0.69033179581025));
#11558=CARTESIAN_POINT('Ctrl Pts',(11.399993839827,-1.36065445462682,0.69228884175444));
#11559=CARTESIAN_POINT('Ctrl Pts',(11.3999946245508,-1.35330733883187,0.695323106179894));
#11560=CARTESIAN_POINT('Ctrl Pts',(11.3999965692242,-1.34565642326237,0.69750197024776));
#11561=CARTESIAN_POINT('Ctrl Pts',(11.3999981510416,-1.33784990929195,0.698756936804364));
#11562=CARTESIAN_POINT('Ctrl Pts',(11.399999182603,-1.33275899381189,0.699575346749464));
#11563=CARTESIAN_POINT('Ctrl Pts',(11.4000000015384,-1.32760128986121,0.699999998642559));
#11564=CARTESIAN_POINT('Ctrl Pts',(11.3999999999682,-1.32241589773435,0.7));
#11565=CARTESIAN_POINT('Ctrl Pts',(11.227882892666,-1.47337141465794,-0.000640335460849732));
#11566=CARTESIAN_POINT('Ctrl Pts',(11.218588765022,-1.46278323638644,0.201451598614313));
#11567=CARTESIAN_POINT('Ctrl Pts',(11.2092944683555,-1.45219508216535,0.40354352620373));
#11568=CARTESIAN_POINT('Ctrl Pts',(11.2000000000001,-1.44160695250309,0.60563544721184));
#11569=CARTESIAN_POINT('Ctrl Pts',(10.1843397214697,-1.57034855377304,-0.000384310983874139));
#11570=CARTESIAN_POINT('Ctrl Pts',(10.1768953195658,-1.55975965902304,0.201708049868595));
#11571=CARTESIAN_POINT('Ctrl Pts',(10.1694507716805,-1.54917076711515,0.403800406245857));
#11572=CARTESIAN_POINT('Ctrl Pts',(10.1620060668616,-1.53858190981164,0.605892758286982));
#11573=CARTESIAN_POINT('Ctrl Pts',(9.14170648965309,-1.65016851777514,-0.000148134864058495));
#11574=CARTESIAN_POINT('Ctrl Pts',(9.13611341817177,-1.63957870617509,0.201944615677573));
#11575=CARTESIAN_POINT('Ctrl Pts',(9.13052023035058,-1.6289888900612,0.404037363603497));
#11576=CARTESIAN_POINT('Ctrl Pts',(9.124926910836,-1.6183991014662,0.606130109186173));
#11577=CARTESIAN_POINT('Ctrl Pts',(8.1,-1.69866351109718,1.00613961606655E-16));
#11578=CARTESIAN_POINT('Ctrl Pts',(8.09625995443094,-1.68807302815665,0.202092993803311));
#11579=CARTESIAN_POINT('Ctrl Pts',(8.09251982249141,-1.67748255132318,0.404185986335255));
#11580=CARTESIAN_POINT('Ctrl Pts',(8.08877960280056,-1.66689208072706,0.606278977577217));
#11581=CARTESIAN_POINT('Ctrl Pts',(8.1,-1.66641703131627,0.605314487869832));
#11582=CARTESIAN_POINT('Ctrl Pts',(9.13548525483003,-1.617718421277,0.605389190939432));
#11583=CARTESIAN_POINT('Ctrl Pts',(10.168822041161,-1.53796707615457,0.605507632815633));
#11584=CARTESIAN_POINT('Ctrl Pts',(11.2000000000893,-1.44160695345912,0.605635447210802));
#11585=CARTESIAN_POINT('Ctrl Pts',(11.7095939787209,-1.42740645209206,-7.69249563980189E-5));
#11586=CARTESIAN_POINT('Ctrl Pts',(11.6994545874061,-1.41682738380082,0.201847033339061));
#11587=CARTESIAN_POINT('Ctrl Pts',(11.6893150192885,-1.40624834198077,0.403770984173611));
#11588=CARTESIAN_POINT('Ctrl Pts',(11.6791752715866,-1.39566932719028,0.605694927437301));
#11589=CARTESIAN_POINT('Ctrl Pts',(11.6063871276792,-1.43748358609578,-5.11721697277706E-5));
#11590=CARTESIAN_POINT('Ctrl Pts',(11.596430427176,-1.42690445239132,0.201872829148883));
#11591=CARTESIAN_POINT('Ctrl Pts',(11.5864735514701,-1.41632534465399,0.403796823219986));
#11592=CARTESIAN_POINT('Ctrl Pts',(11.5765164978042,-1.40574626343445,0.605720809936841));
#11593=CARTESIAN_POINT('Ctrl Pts',(11.5031891278894,-1.4474144288224,-2.55082377288765E-5));
#11594=CARTESIAN_POINT('Ctrl Pts',(11.4934151336386,-1.43683522760458,0.201898535909597));
#11595=CARTESIAN_POINT('Ctrl Pts',(11.4836409658656,-1.42625605183456,0.40382257302165));
#11596=CARTESIAN_POINT('Ctrl Pts',(11.4738666218385,-1.41567690205216,0.605746602994839));
#11597=CARTESIAN_POINT('Ctrl Pts',(11.4,-1.45718524058191,-5.20417042793042E-18));
#11598=CARTESIAN_POINT('Ctrl Pts',(11.3904087275488,-1.44660597001679,0.201924086674796));
#11599=CARTESIAN_POINT('Ctrl Pts',(11.3808172833376,-1.43602672436683,0.403848166524883));
#11600=CARTESIAN_POINT('Ctrl Pts',(11.3712256646606,-1.42544750415802,0.605772239449758));
#11601=CARTESIAN_POINT('',(11.6778970386953,-1.39579479040469,0.605695249702977));
#11602=CARTESIAN_POINT('Ctrl Pts',(11.4,-1.4227102204299,0.605660349289938));
#11603=CARTESIAN_POINT('Ctrl Pts',(11.4926474653491,-1.41386220753305,0.605671932550561));
#11604=CARTESIAN_POINT('Ctrl Pts',(11.585279512325,-1.40488700096013,0.605683574233495));
#11605=CARTESIAN_POINT('Ctrl Pts',(11.6778970386953,-1.39579479040469,0.605695249702977));
#11606=CARTESIAN_POINT('Ctrl Pts',(11.6778970386953,-1.39579479040469,0.605695249702977));
#11607=CARTESIAN_POINT('Ctrl Pts',(11.6884613130147,-1.40633044792991,0.403796817797553));
#11608=CARTESIAN_POINT('Ctrl Pts',(11.6990256725537,-1.41686632615463,0.201898401304098));
#11609=CARTESIAN_POINT('Ctrl Pts',(11.7095901160181,-1.42740242188993,5.19332840620557E-17));
#11610=CARTESIAN_POINT('Ctrl Pts',(11.2,-1.34133050917871,0.7));
#11611=CARTESIAN_POINT('Ctrl Pts',(10.1668086441106,-1.43797263608903,0.7));
#11612=CARTESIAN_POINT('Ctrl Pts',(9.13190264019122,-1.51792184128158,0.7));
#11613=CARTESIAN_POINT('Ctrl Pts',(8.09530923905977,-1.56666858280461,0.7));
#11614=CARTESIAN_POINT('Ctrl Pts',(11.2026864299662,-1.37005086445236,0.7));
#11615=CARTESIAN_POINT('Ctrl Pts',(10.1691860218014,-1.46674693471719,0.700000910790016));
#11616=CARTESIAN_POINT('Ctrl Pts',(9.13384227773975,-1.54675516497,0.699999464833944));
#11617=CARTESIAN_POINT('Ctrl Pts',(8.09666712422266,-1.59554384206015,0.700000000000001));
#11618=CARTESIAN_POINT('Ctrl Pts',(11.2073428085028,-1.4198317437391,0.676744232988519));
#11619=CARTESIAN_POINT('Ctrl Pts',(10.1733099382853,-1.51661799675652,0.676702307311825));
#11620=CARTESIAN_POINT('Ctrl Pts',(9.13719745543551,-1.59672983278297,0.676663906627884));
#11621=CARTESIAN_POINT('Ctrl Pts',(8.09902054834098,-1.64558911349573,0.676639354455264));
#11622=CARTESIAN_POINT('Ctrl Pts',(11.2091847227485,-1.43952346553595,0.627236497176141));
#11623=CARTESIAN_POINT('Ctrl Pts',(10.1749352046592,-1.53629892039422,0.62712791425818));
#11624=CARTESIAN_POINT('Ctrl Pts',(9.13852107143019,-1.61640633519008,0.627027713743691));
#11625=CARTESIAN_POINT('Ctrl Pts',(8.0999458765183,-1.66526610220338,0.626964226563296));
#11626=CARTESIAN_POINT('Ctrl Pts',(11.209298290232,-1.4407376041935,0.605636599993194));
#11627=CARTESIAN_POINT('Ctrl Pts',(10.1750338985877,-1.53748737250229,0.605508345221004));
#11628=CARTESIAN_POINT('Ctrl Pts',(9.13859765097935,-1.61757204607208,0.605389415477198));
#11629=CARTESIAN_POINT('Ctrl Pts',(8.1,-1.66641703131627,0.605314487869832));
#11630=CARTESIAN_POINT('Ctrl Pts',(11.2,-1.34133050917871,0.7));
#11631=CARTESIAN_POINT('Ctrl Pts',(10.16836710286,-1.43782686176815,0.7));
#11632=CARTESIAN_POINT('Ctrl Pts',(9.13502472651537,-1.51768061363633,0.7));
#11633=CARTESIAN_POINT('Ctrl Pts',(8.09999999865516,-1.56644778212326,0.7));
#11634=CARTESIAN_POINT('Ctrl Pts',(11.6681436286308,-1.2964346619681,0.7));
#11635=CARTESIAN_POINT('Ctrl Pts',(11.5756099286391,-1.3055179747114,0.7));
#11636=CARTESIAN_POINT('Ctrl Pts',(11.4830653488871,-1.31448403714215,0.7));
#11637=CARTESIAN_POINT('Ctrl Pts',(11.3905090053564,-1.32332268868375,0.7));
#11638=CARTESIAN_POINT('Ctrl Pts',(11.6709605510772,-1.32513126902304,0.700000000000001));
#11639=CARTESIAN_POINT('Ctrl Pts',(11.5784027531871,-1.33421922733773,0.700000082825348));
#11640=CARTESIAN_POINT('Ctrl Pts',(11.4858332859074,-1.34318985044544,0.699999917777441));
#11641=CARTESIAN_POINT('Ctrl Pts',(11.3932507170007,-1.35203326785046,0.7));
#11642=CARTESIAN_POINT('Ctrl Pts',(11.6758431636759,-1.37487151491717,0.67676311428296));
#11643=CARTESIAN_POINT('Ctrl Pts',(11.583243842395,-1.38396722707511,0.676759299309384));
#11644=CARTESIAN_POINT('Ctrl Pts',(11.4906306781253,-1.39294591144353,0.676755553516685));
#11645=CARTESIAN_POINT('Ctrl Pts',(11.3980029235659,-1.40179729139028,0.67675176769038));
#11646=CARTESIAN_POINT('Ctrl Pts',(11.6777767156198,-1.39456903283364,0.627286048421068));
#11647=CARTESIAN_POINT('Ctrl Pts',(11.5851604051362,-1.40366358810601,0.627276165220861));
#11648=CARTESIAN_POINT('Ctrl Pts',(11.4925297866457,-1.41264104586547,0.627266369072496));
#11649=CARTESIAN_POINT('Ctrl Pts',(11.3998836071583,-1.4214913811319,0.627256563056779));
#11650=CARTESIAN_POINT('Ctrl Pts',(11.6778970386953,-1.39579479040469,0.605695249702977));
#11651=CARTESIAN_POINT('Ctrl Pts',(11.585279512325,-1.40488700096013,0.605683574233495));
#11652=CARTESIAN_POINT('Ctrl Pts',(11.4926474653491,-1.41386220753305,0.605671932550561));
#11653=CARTESIAN_POINT('Ctrl Pts',(11.4,-1.4227102204299,0.605660349289938));
#11654=CARTESIAN_POINT('',(11.6681436286308,-1.2964346619681,0.7));
#11655=CARTESIAN_POINT('Ctrl Pts',(11.6681436286308,-1.2964346619681,0.7));
#11656=CARTESIAN_POINT('Ctrl Pts',(11.5787728332608,-1.30520749699507,0.7));
#11657=CARTESIAN_POINT('Ctrl Pts',(11.4893918891838,-1.31387096021207,0.7));
#11658=CARTESIAN_POINT('Ctrl Pts',(11.3999999999682,-1.32241589773435,0.7));
#11659=CARTESIAN_POINT('Origin',(11.6681436286308,-1.2964346619681,0.6));
#11660=CARTESIAN_POINT('Origin',(6.08012166120517,1.06778195214465E-16,
0.7));
#11661=CARTESIAN_POINT('Ctrl Pts',(8.0999999986552,1.56644778212326,0.7));
#11662=CARTESIAN_POINT('Ctrl Pts',(9.13502472651542,1.51768061363633,0.7));
#11663=CARTESIAN_POINT('Ctrl Pts',(10.16836710286,1.43782686176815,0.7));
#11664=CARTESIAN_POINT('Ctrl Pts',(11.2,1.34133050917871,0.7));
#11665=CARTESIAN_POINT('Origin',(6.08012166120517,1.06778195214465E-16,
0.7));
#11666=CARTESIAN_POINT('',(11.6681436286308,1.2964346619681,0.7));
#11667=CARTESIAN_POINT('Ctrl Pts',(11.3999999999682,1.32241589773435,0.7));
#11668=CARTESIAN_POINT('Ctrl Pts',(11.4893918891837,1.31387096021208,0.7));
#11669=CARTESIAN_POINT('Ctrl Pts',(11.5787728332608,1.30520749699508,0.7));
#11670=CARTESIAN_POINT('Ctrl Pts',(11.6681436286308,1.2964346619681,0.7));
#11671=CARTESIAN_POINT('',(11.6681436286308,0.8,0.7));
#11672=CARTESIAN_POINT('Ctrl Pts',(8.09530923905978,1.56666858280461,0.7));
#11673=CARTESIAN_POINT('Ctrl Pts',(9.13190264019124,1.51792184128158,0.7));
#11674=CARTESIAN_POINT('Ctrl Pts',(10.1668086441106,1.43797263608903,0.7));
#11675=CARTESIAN_POINT('Ctrl Pts',(11.2,1.34133050917871,0.7));
#11676=CARTESIAN_POINT('Ctrl Pts',(8.09666712422266,1.59554384206015,0.700000000000001));
#11677=CARTESIAN_POINT('Ctrl Pts',(9.13384227773977,1.54675516497,0.699999464833944));
#11678=CARTESIAN_POINT('Ctrl Pts',(10.1691860218013,1.46674693471719,0.700000910790016));
#11679=CARTESIAN_POINT('Ctrl Pts',(11.2026864299662,1.37005086445236,0.7));
#11680=CARTESIAN_POINT('Ctrl Pts',(8.09902054834099,1.64558911349573,0.676639354455264));
#11681=CARTESIAN_POINT('Ctrl Pts',(9.13719745543553,1.59672983278297,0.676663906627884));
#11682=CARTESIAN_POINT('Ctrl Pts',(10.1733099382853,1.51661799675652,0.676702307311825));
#11683=CARTESIAN_POINT('Ctrl Pts',(11.2073428085028,1.4198317437391,0.676744232988519));
#11684=CARTESIAN_POINT('Ctrl Pts',(8.0999458765183,1.66526610220338,0.626964226563296));
#11685=CARTESIAN_POINT('Ctrl Pts',(9.1385210714302,1.61640633519008,0.627027713743691));
#11686=CARTESIAN_POINT('Ctrl Pts',(10.1749352046592,1.53629892039423,0.62712791425818));
#11687=CARTESIAN_POINT('Ctrl Pts',(11.2091847227485,1.43952346553595,0.627236497176141));
#11688=CARTESIAN_POINT('Ctrl Pts',(8.1,1.66641703131627,0.605314487869832));
#11689=CARTESIAN_POINT('Ctrl Pts',(9.13859765097937,1.61757204607208,0.605389415477198));
#11690=CARTESIAN_POINT('Ctrl Pts',(10.1750338985877,1.53748737250229,0.605508345221004));
#11691=CARTESIAN_POINT('Ctrl Pts',(11.209298290232,1.4407376041935,0.605636599993194));
#11692=CARTESIAN_POINT('Ctrl Pts',(11.2000000000893,1.44160695345912,0.605635447210802));
#11693=CARTESIAN_POINT('Ctrl Pts',(10.168822041161,1.53796707615457,0.605507632815633));
#11694=CARTESIAN_POINT('Ctrl Pts',(9.13548525483005,1.617718421277,0.605389190939432));
#11695=CARTESIAN_POINT('Ctrl Pts',(8.1,1.66641703131627,0.605314487869832));
#11696=CARTESIAN_POINT('Ctrl Pts',(8.1,1.69866351109859,-2.6441702993818E-11));
#11697=CARTESIAN_POINT('Ctrl Pts',(8.09625995443078,1.68807302815759,0.202092993785684));
#11698=CARTESIAN_POINT('Ctrl Pts',(8.09251982249108,1.67748255132366,0.404185986326441));
#11699=CARTESIAN_POINT('Ctrl Pts',(8.08877960280008,1.66689208072708,0.606278977577217));
#11700=CARTESIAN_POINT('Ctrl Pts',(9.14170648965349,1.65016851777655,-0.00014813489050026));
#11701=CARTESIAN_POINT('Ctrl Pts',(9.13611341817193,1.63957870617604,0.201944615659945));
#11702=CARTESIAN_POINT('Ctrl Pts',(9.1305202303505,1.62898889006169,0.404037363594684));
#11703=CARTESIAN_POINT('Ctrl Pts',(9.12492691083567,1.61839910146622,0.606130109186173));
#11704=CARTESIAN_POINT('Ctrl Pts',(10.1843397214705,1.57034855377444,-0.000384311010315772));
#11705=CARTESIAN_POINT('Ctrl Pts',(10.1768953195662,1.55975965902398,0.201708049850968));
#11706=CARTESIAN_POINT('Ctrl Pts',(10.1694507716807,1.54917076711562,0.403800406237042));
#11707=CARTESIAN_POINT('Ctrl Pts',(10.1620060668615,1.53858190981166,0.605892758286982));
#11708=CARTESIAN_POINT('Ctrl Pts',(11.2278828926672,1.47337141465933,-0.000640335487291374));
#11709=CARTESIAN_POINT('Ctrl Pts',(11.2185887650228,1.46278323638736,0.201451598596686));
#11710=CARTESIAN_POINT('Ctrl Pts',(11.2092944683559,1.45219508216582,0.403543526194916));
#11711=CARTESIAN_POINT('Ctrl Pts',(11.2000000000001,1.44160695250309,0.60563544721184));
#11712=CARTESIAN_POINT('Ctrl Pts',(11.4,1.45718524058191,-1.37043154602168E-16));
#11713=CARTESIAN_POINT('Ctrl Pts',(11.3904087275488,1.44660597001679,0.201924086674796));
#11714=CARTESIAN_POINT('Ctrl Pts',(11.3808172833376,1.43602672436683,0.403848166524884));
#11715=CARTESIAN_POINT('Ctrl Pts',(11.3712256646606,1.42544750415802,0.605772239449759));
#11716=CARTESIAN_POINT('Ctrl Pts',(11.5031891278894,1.4474144288224,-2.55082377290153E-5));
#11717=CARTESIAN_POINT('Ctrl Pts',(11.4934151336386,1.43683522760458,0.201898535909598));
#11718=CARTESIAN_POINT('Ctrl Pts',(11.4836409658656,1.42625605183455,0.40382257302165));
#11719=CARTESIAN_POINT('Ctrl Pts',(11.4738666218385,1.41567690205216,0.605746602994839));
#11720=CARTESIAN_POINT('Ctrl Pts',(11.6063871276792,1.43748358609579,-5.1172169727805E-5));
#11721=CARTESIAN_POINT('Ctrl Pts',(11.596430427176,1.42690445239132,0.201872829148883));
#11722=CARTESIAN_POINT('Ctrl Pts',(11.5864735514701,1.41632534465399,0.403796823219986));
#11723=CARTESIAN_POINT('Ctrl Pts',(11.5765164978042,1.40574626343445,0.605720809936842));
#11724=CARTESIAN_POINT('Ctrl Pts',(11.7095939787209,1.42740645209206,-7.69249563980588E-5));
#11725=CARTESIAN_POINT('Ctrl Pts',(11.6994545874061,1.41682738380082,0.201847033339061));
#11726=CARTESIAN_POINT('Ctrl Pts',(11.6893150192885,1.40624834198077,0.403770984173611));
#11727=CARTESIAN_POINT('Ctrl Pts',(11.6791752715866,1.39566932719028,0.605694927437301));
#11728=CARTESIAN_POINT('',(11.6778970386953,1.39579479040469,0.605695249702977));
#11729=CARTESIAN_POINT('Ctrl Pts',(11.7095901160181,1.42740242188993,2.01986864734049E-16));
#11730=CARTESIAN_POINT('Ctrl Pts',(11.6990256725537,1.41686632615463,0.201898401304098));
#11731=CARTESIAN_POINT('Ctrl Pts',(11.6884613130147,1.40633044792991,0.403796817797553));
#11732=CARTESIAN_POINT('Ctrl Pts',(11.6778970386953,1.39579479040469,0.605695249702978));
#11733=CARTESIAN_POINT('Ctrl Pts',(11.6778970386953,1.39579479040469,0.605695249702977));
#11734=CARTESIAN_POINT('Ctrl Pts',(11.585279512325,1.40488700096013,0.605683574233495));
#11735=CARTESIAN_POINT('Ctrl Pts',(11.4926474653491,1.41386220753305,0.605671932550561));
#11736=CARTESIAN_POINT('Ctrl Pts',(11.4,1.4227102204299,0.605660349289938));
#11737=CARTESIAN_POINT('Origin',(7.9,1.7737037037037,0.));
#11738=CARTESIAN_POINT('',(7.9,-1.67543132363858,0.605300614462415));
#11739=CARTESIAN_POINT('Ctrl Pts',(7.9,-1.67543132363858,0.605300614462415));
#11740=CARTESIAN_POINT('Ctrl Pts',(7.9,-1.68078196203297,0.504592238472094));
#11741=CARTESIAN_POINT('Ctrl Pts',(7.9,-1.68613236521525,0.403883028813119));
#11742=CARTESIAN_POINT('Ctrl Pts',(7.9,-1.69685110017509,0.202116711316755));
#11743=CARTESIAN_POINT('Ctrl Pts',(7.9,-1.70221951791351,0.10105794916591));
#11744=CARTESIAN_POINT('Ctrl Pts',(7.9,-1.70758761671949,0.));
#11745=CARTESIAN_POINT('',(7.9,-1.57547905376932,0.7));
#11746=CARTESIAN_POINT('Ctrl Pts',(7.9,-1.57547905376882,0.7));
#11747=CARTESIAN_POINT('Ctrl Pts',(7.9,-1.58339333479856,0.700000000000001));
#11748=CARTESIAN_POINT('Ctrl Pts',(7.89999913038498,-1.59124411312484,0.699006032637452));
#11749=CARTESIAN_POINT('Ctrl Pts',(7.89999837104309,-1.59889106951376,0.697118831203047));
#11750=CARTESIAN_POINT('Ctrl Pts',(7.89999794343345,-1.6031973145812,0.696056087876834));
#11751=CARTESIAN_POINT('Ctrl Pts',(7.89999755365678,-1.60743898057435,0.694709047589066));
#11752=CARTESIAN_POINT('Ctrl Pts',(7.89999730661842,-1.61158931211603,0.693088720937666));
#11753=CARTESIAN_POINT('Ctrl Pts',(7.89999686465941,-1.6190143793929,0.690189908089508));
#11754=CARTESIAN_POINT('Ctrl Pts',(7.89999696143539,-1.626066934352,0.686450944759811));
#11755=CARTESIAN_POINT('Ctrl Pts',(7.89999752554231,-1.63260082031789,0.681953255064161));
#11756=CARTESIAN_POINT('Ctrl Pts',(7.89999783650325,-1.63620259020663,0.679473927540052));
#11757=CARTESIAN_POINT('Ctrl Pts',(7.89999827825103,-1.63964648551863,0.676763160200805));
#11758=CARTESIAN_POINT('Ctrl Pts',(7.89999867021687,-1.64290407802379,0.673829034208746));
#11759=CARTESIAN_POINT('Ctrl Pts',(7.89999905115172,-1.64606999298761,0.670977482527793));
#11760=CARTESIAN_POINT('Ctrl Pts',(7.89999938859403,-1.64904076201529,0.667932171841817));
#11761=CARTESIAN_POINT('Ctrl Pts',(7.89999938783828,-1.6517939440564,0.66470449824639));
#11762=CARTESIAN_POINT('Ctrl Pts',(7.89999938643498,-1.65690611124346,0.658711285012161));
#11763=CARTESIAN_POINT('Ctrl Pts',(7.89999834643869,-1.661271022418,0.652090721578155));
#11764=CARTESIAN_POINT('Ctrl Pts',(7.89999799057748,-1.66482884904143,0.645008203309728));
#11765=CARTESIAN_POINT('Ctrl Pts',(7.89999795399159,-1.66519462718329,0.644280053614395));
#11766=CARTESIAN_POINT('Ctrl Pts',(7.89999792287445,-1.66555183396469,0.643547001244109));
#11767=CARTESIAN_POINT('Ctrl Pts',(7.89999789784292,-1.66590037542058,0.642809214685104));
#11768=CARTESIAN_POINT('Ctrl Pts',(7.89999765441981,-1.66928982250308,0.635634491398386));
#11769=CARTESIAN_POINT('Ctrl Pts',(7.89999817709027,-1.67182454272713,0.628096763436417));
#11770=CARTESIAN_POINT('Ctrl Pts',(7.8999989464625,-1.67345106343068,0.620364350320046));
#11771=CARTESIAN_POINT('Ctrl Pts',(7.89999943944948,-1.67449328136075,0.615409688768565));
#11772=CARTESIAN_POINT('Ctrl Pts',(7.89999999630063,-1.67516175160204,0.610374426093907));
#11773=CARTESIAN_POINT('Ctrl Pts',(7.89999999769359,-1.67543132314592,0.605300614465834));
#11774=CARTESIAN_POINT('',(7.9,1.57547905376882,0.7));
#11775=CARTESIAN_POINT('',(7.9,0.886851851851852,0.7));
#11776=CARTESIAN_POINT('',(7.9,1.67543132363858,0.605300614462415));
#11777=CARTESIAN_POINT('Ctrl Pts',(7.89999999769359,1.67543132314592,0.605300614465834));
#11778=CARTESIAN_POINT('Ctrl Pts',(7.89999999552123,1.67501091691767,0.613213400729193));
#11779=CARTESIAN_POINT('Ctrl Pts',(7.89999875799714,1.67362284400845,0.621034919585595));
#11780=CARTESIAN_POINT('Ctrl Pts',(7.89999821041927,1.67135120200026,0.628604813990272));
#11781=CARTESIAN_POINT('Ctrl Pts',(7.89999790518813,1.67008494211401,0.632824428521627));
#11782=CARTESIAN_POINT('Ctrl Pts',(7.89999777089825,1.66854314417455,0.636965893954691));
#11783=CARTESIAN_POINT('Ctrl Pts',(7.89999784944871,1.66673368022774,0.640999456224326));
#11784=CARTESIAN_POINT('Ctrl Pts',(7.89999799035603,1.66348778281681,0.648235040746992));
#11785=CARTESIAN_POINT('Ctrl Pts',(7.8999989183875,1.65941887886545,0.655045206964536));
#11786=CARTESIAN_POINT('Ctrl Pts',(7.89999927807636,1.65459101651367,0.661266862646797));
#11787=CARTESIAN_POINT('Ctrl Pts',(7.89999934554656,1.65368540929837,0.662433916689859));
#11788=CARTESIAN_POINT('Ctrl Pts',(7.89999938740919,1.65275296801062,0.663580193269421));
#11789=CARTESIAN_POINT('Ctrl Pts',(7.89999938728957,1.65179394408007,0.664704498246374));
#11790=CARTESIAN_POINT('Ctrl Pts',(7.89999938705343,1.64990069294102,0.666924037937161));
#11791=CARTESIAN_POINT('Ctrl Pts',(7.89999922461202,1.64790387543569,0.669057997255949));
#11792=CARTESIAN_POINT('Ctrl Pts',(7.89999900301747,1.64581073954063,0.671102663899023));
#11793=CARTESIAN_POINT('Ctrl Pts',(7.89999840121276,1.64012621790684,0.676655553128015));
#11794=CARTESIAN_POINT('Ctrl Pts',(7.89999746538644,1.63379824275617,0.681490110487894));
#11795=CARTESIAN_POINT('Ctrl Pts',(7.89999715581736,1.6269906793715,0.685552192443336));
#11796=CARTESIAN_POINT('Ctrl Pts',(7.89999695885968,1.62265949106942,0.688136618155352));
#11797=CARTESIAN_POINT('Ctrl Pts',(7.89999697413705,1.61813320929371,0.690407672840119));
#11798=CARTESIAN_POINT('Ctrl Pts',(7.89999720528031,1.61344832872307,0.692342105328139));
#11799=CARTESIAN_POINT('Ctrl Pts',(7.89999756646959,1.60612763680413,0.69536488980882));
#11800=CARTESIAN_POINT('Ctrl Pts',(7.89999845750109,1.59850458633822,0.69753330980446));
#11801=CARTESIAN_POINT('Ctrl Pts',(7.89999917312139,1.59072625322659,0.698777780766876));
#11802=CARTESIAN_POINT('Ctrl Pts',(7.8999996358458,1.58569673594883,0.699582463224842));
#11803=CARTESIAN_POINT('Ctrl Pts',(7.9,1.58060170040825,0.7));
#11804=CARTESIAN_POINT('Ctrl Pts',(7.9,1.57547905376882,0.7));
#11805=CARTESIAN_POINT('Ctrl Pts',(7.9,1.70758761671949,0.));
#11806=CARTESIAN_POINT('Ctrl Pts',(7.9,1.70221949782947,0.101058327261027));
#11807=CARTESIAN_POINT('Ctrl Pts',(7.9,1.69685105999395,0.202117467714));
#11808=CARTESIAN_POINT('Ctrl Pts',(7.9,1.68613232500772,0.403883785628764));
#11809=CARTESIAN_POINT('Ctrl Pts',(7.9,1.6807819419292,0.504592616860323));
#11810=CARTESIAN_POINT('Ctrl Pts',(7.9,1.67543132363858,0.605300614462415));
#11811=CARTESIAN_POINT('Ctrl Pts',(7.91019312999368,-1.70715886092982,-0.000134090250286965));
#11812=CARTESIAN_POINT('Ctrl Pts',(7.90679525219671,-1.69658223918655,0.201692187253877));
#11813=CARTESIAN_POINT('Ctrl Pts',(7.90339729501941,-1.68600562260833,0.40351846369823));
#11814=CARTESIAN_POINT('Ctrl Pts',(7.89999925719352,-1.67542901130525,0.605344739067286));
#11815=CARTESIAN_POINT('Ctrl Pts',(6.63535348802246,-1.76179300886274,3.38453142643293E-5));
#11816=CARTESIAN_POINT('Ctrl Pts',(6.63422081661327,-1.7512156246026,0.201860399405878));
#11817=CARTESIAN_POINT('Ctrl Pts',(6.6330881724013,-1.74063821514668,0.403686949685767));
#11818=CARTESIAN_POINT('Ctrl Pts',(6.63195543348167,-1.7300608292057,0.605513504373875));
#11819=CARTESIAN_POINT('Ctrl Pts',(5.36191629096386,-1.76821426310706,6.25694230841134E-5));
#11820=CARTESIAN_POINT('Ctrl Pts',(5.36305144950513,-1.75763653444312,0.201889164820622));
#11821=CARTESIAN_POINT('Ctrl Pts',(5.36418670601529,-1.74705878452761,0.403715755186214));
#11822=CARTESIAN_POINT('Ctrl Pts',(5.36532191986746,-1.73648104871457,0.605542351516859));
#11823=CARTESIAN_POINT('Ctrl Pts',(4.08978435919194,-1.70060618495018,-0.000163379468877527));
#11824=CARTESIAN_POINT('Ctrl Pts',(4.09318947412453,-1.69002991101751,0.201662855819258));
#11825=CARTESIAN_POINT('Ctrl Pts',(4.09659468720556,-1.67945364498778,0.403489089874722));
#11826=CARTESIAN_POINT('Ctrl Pts',(4.1,-1.66887738702936,0.605315322680078));
#11827=CARTESIAN_POINT('Ctrl Pts',(4.10000000006189,-1.66887738587128,0.605315322687833));
#11828=CARTESIAN_POINT('Ctrl Pts',(5.36600428635239,-1.73653511802878,0.605201749988751));
#11829=CARTESIAN_POINT('Ctrl Pts',(6.63469107356441,-1.72995836404769,0.605216415547347));
#11830=CARTESIAN_POINT('Ctrl Pts',(7.89999999997453,-1.67543132304763,0.605300614465986));
#11831=CARTESIAN_POINT('Ctrl Pts',(7.9,-1.57547905376882,0.7));
#11832=CARTESIAN_POINT('Ctrl Pts',(6.63400208894818,-1.63014048526579,0.7));
#11833=CARTESIAN_POINT('Ctrl Pts',(5.36531976402288,-1.63670020240541,0.7));
#11834=CARTESIAN_POINT('Ctrl Pts',(4.09999999999999,-1.56887583540973,0.7));
#11835=CARTESIAN_POINT('Ctrl Pts',(7.9012470621039,-1.60436190544783,0.700000000000001));
#11836=CARTESIAN_POINT('Ctrl Pts',(6.6345175325877,-1.65907137725265,0.700000604190856));
#11837=CARTESIAN_POINT('Ctrl Pts',(5.36490325870521,-1.66564852467601,0.700000815814724));
#11838=CARTESIAN_POINT('Ctrl Pts',(4.09845273665223,-1.59774131518914,0.699999999999999));
#11839=CARTESIAN_POINT('Ctrl Pts',(7.90340849276168,-1.6544221878571,0.676636720659303));
#11840=CARTESIAN_POINT('Ctrl Pts',(6.63541917043928,-1.70921256696412,0.676609005714152));
#11841=CARTESIAN_POINT('Ctrl Pts',(5.36416860778507,-1.71581908642683,0.67660414986632));
#11842=CARTESIAN_POINT('Ctrl Pts',(4.09577098158984,-1.64777167791894,0.676641578059328));
#11843=CARTESIAN_POINT('Ctrl Pts',(7.90425799286387,-1.67409721877663,0.626952737571144));
#11844=CARTESIAN_POINT('Ctrl Pts',(6.63576820027036,-1.72888861107585,0.626881076846221));
#11845=CARTESIAN_POINT('Ctrl Pts',(5.36388821219926,-1.73550154452763,0.626868555890157));
#11846=CARTESIAN_POINT('Ctrl Pts',(4.09471668402893,-1.66744047248441,0.626965338598652));
#11847=CARTESIAN_POINT('Ctrl Pts',(7.90430757201307,-1.67524550738887,0.605300901379154));
#11848=CARTESIAN_POINT('Ctrl Pts',(6.63578978311492,-1.73002023206136,0.605216330280387));
#11849=CARTESIAN_POINT('Ctrl Pts',(5.3638700255334,-1.7366305488338,0.605201579557148));
#11850=CARTESIAN_POINT('Ctrl Pts',(4.09465499692593,-1.6685912965035,0.605315802949303));
#11851=CARTESIAN_POINT('Ctrl Pts',(7.9,-1.57547905376882,0.7));
#11852=CARTESIAN_POINT('Ctrl Pts',(6.63400208894818,-1.63014048526579,0.7));
#11853=CARTESIAN_POINT('Ctrl Pts',(5.36531976402288,-1.63670020240541,0.7));
#11854=CARTESIAN_POINT('Ctrl Pts',(4.09999999999999,-1.56887583540973,0.7));
#11855=CARTESIAN_POINT('Origin',(6.08012166120517,1.06778195214465E-16,
0.7));
#11856=CARTESIAN_POINT('Ctrl Pts',(4.1,1.56887583540973,0.7));
#11857=CARTESIAN_POINT('Ctrl Pts',(5.36531976402291,1.63670020240541,0.7));
#11858=CARTESIAN_POINT('Ctrl Pts',(6.63400208894819,1.63014048526579,0.7));
#11859=CARTESIAN_POINT('Ctrl Pts',(7.9,1.57547905376882,0.7));
#11860=CARTESIAN_POINT('Ctrl Pts',(4.1,1.56887583540973,0.7));
#11861=CARTESIAN_POINT('Ctrl Pts',(5.36531976402291,1.63670020240541,0.7));
#11862=CARTESIAN_POINT('Ctrl Pts',(6.63400208894819,1.63014048526579,0.7));
#11863=CARTESIAN_POINT('Ctrl Pts',(7.9,1.57547905376882,0.7));
#11864=CARTESIAN_POINT('Ctrl Pts',(4.09845273665224,1.59774131518914,0.699999999999999));
#11865=CARTESIAN_POINT('Ctrl Pts',(5.36490325870523,1.66564852467601,0.700000815814725));
#11866=CARTESIAN_POINT('Ctrl Pts',(6.6345175325877,1.65907137725265,0.700000604190856));
#11867=CARTESIAN_POINT('Ctrl Pts',(7.9012470621039,1.60436190544783,0.700000000000001));
#11868=CARTESIAN_POINT('Ctrl Pts',(4.09577098158985,1.64777167791894,0.676641578059328));
#11869=CARTESIAN_POINT('Ctrl Pts',(5.36416860778509,1.71581908642683,0.67660414986632));
#11870=CARTESIAN_POINT('Ctrl Pts',(6.6354191704393,1.70921256696412,0.676609005714152));
#11871=CARTESIAN_POINT('Ctrl Pts',(7.90340849276168,1.6544221878571,0.676636720659302));
#11872=CARTESIAN_POINT('Ctrl Pts',(4.09471668402895,1.66744047248441,0.626965338598652));
#11873=CARTESIAN_POINT('Ctrl Pts',(5.36388821219928,1.73550154452763,0.626868555890157));
#11874=CARTESIAN_POINT('Ctrl Pts',(6.63576820027036,1.72888861107585,0.626881076846221));
#11875=CARTESIAN_POINT('Ctrl Pts',(7.90425799286387,1.67409721877663,0.626952737571144));
#11876=CARTESIAN_POINT('Ctrl Pts',(4.09465499692594,1.6685912965035,0.605315802949303));
#11877=CARTESIAN_POINT('Ctrl Pts',(5.36387002553342,1.7366305488338,0.605201579557148));
#11878=CARTESIAN_POINT('Ctrl Pts',(6.63578978311492,1.73002023206136,0.605216330280387));
#11879=CARTESIAN_POINT('Ctrl Pts',(7.90430757201307,1.67524550738887,0.605300901379154));
#11880=CARTESIAN_POINT('Ctrl Pts',(7.89999999997454,1.67543132304763,0.605300614465986));
#11881=CARTESIAN_POINT('Ctrl Pts',(6.63469107356441,1.72995836404769,0.605216415547348));
#11882=CARTESIAN_POINT('Ctrl Pts',(5.36600428635241,1.73653511802878,0.605201749988751));
#11883=CARTESIAN_POINT('Ctrl Pts',(4.10000000006189,1.66887738587128,0.605315322687833));
#11884=CARTESIAN_POINT('Ctrl Pts',(4.08978435969213,1.70060618339657,-0.000163349821525811));
#11885=CARTESIAN_POINT('Ctrl Pts',(4.093189474458,1.69002990998177,0.201662875584159));
#11886=CARTESIAN_POINT('Ctrl Pts',(4.0965946873723,1.67945364446992,0.403489099757173));
#11887=CARTESIAN_POINT('Ctrl Pts',(4.1,1.66887738702936,0.605315322680078));
#11888=CARTESIAN_POINT('Ctrl Pts',(5.36191629113061,1.76821426155324,6.25990704884337E-5));
#11889=CARTESIAN_POINT('Ctrl Pts',(5.3630514496163,1.75763653340724,0.201889184585558));
#11890=CARTESIAN_POINT('Ctrl Pts',(5.36418670607087,1.74705878400967,0.403715765068683));
#11891=CARTESIAN_POINT('Ctrl Pts',(5.36532191986745,1.73648104871457,0.605542351516858));
#11892=CARTESIAN_POINT('Ctrl Pts',(6.63535348785608,1.76179300730897,3.38749616628245E-5));
#11893=CARTESIAN_POINT('Ctrl Pts',(6.63422081650235,1.75121562356675,0.20186041917081));
#11894=CARTESIAN_POINT('Ctrl Pts',(6.63308817234583,1.74063821462875,0.403686959568233));
#11895=CARTESIAN_POINT('Ctrl Pts',(6.63195543348166,1.7300608292057,0.605513504373875));
#11896=CARTESIAN_POINT('Ctrl Pts',(7.91019312949454,1.70715885937616,-0.000134060602928919));
#11897=CARTESIAN_POINT('Ctrl Pts',(7.90679525186394,1.69658223815078,0.201692207018782));
#11898=CARTESIAN_POINT('Ctrl Pts',(7.90339729485302,1.68600562209044,0.403518473580683));
#11899=CARTESIAN_POINT('Ctrl Pts',(7.89999925719352,1.67542901130525,0.605344739067286));
#11900=CARTESIAN_POINT('Origin',(3.9,1.7662962962963,0.));
#11901=CARTESIAN_POINT('',(3.9,-1.657567947596,0.605334330700044));
#11902=CARTESIAN_POINT('Ctrl Pts',(3.9,-1.657567947596,0.605334330700044));
#11903=CARTESIAN_POINT('Ctrl Pts',(3.9,-1.66295505583237,0.504667750148195));
#11904=CARTESIAN_POINT('Ctrl Pts',(3.9,-1.66834175427306,0.404000185805616));
#11905=CARTESIAN_POINT('Ctrl Pts',(3.9,-1.67913790341918,0.202222727053817));
#11906=CARTESIAN_POINT('Ctrl Pts',(3.9,-1.68454745406112,0.101110889248462));
#11907=CARTESIAN_POINT('Ctrl Pts',(3.9,-1.68995649764597,0.));
#11908=CARTESIAN_POINT('',(3.9,-1.55753217754889,0.7));
#11909=CARTESIAN_POINT('Ctrl Pts',(3.89999999700315,-1.55753217437,0.7));
#11910=CARTESIAN_POINT('Ctrl Pts',(3.89999999197785,-1.56545359401377,0.699999998841372));
#11911=CARTESIAN_POINT('Ctrl Pts',(3.90000117861029,-1.57331197233837,0.699006163267487));
#11912=CARTESIAN_POINT('Ctrl Pts',(3.90000221019459,-1.58096665047841,0.697118921400131));
#11913=CARTESIAN_POINT('Ctrl Pts',(3.90000279139136,-1.58527931230009,0.696055645348449));
#11914=CARTESIAN_POINT('Ctrl Pts',(3.90000331912093,-1.58952737074567,0.694707745526415));
#11915=CARTESIAN_POINT('Ctrl Pts',(3.90000364796674,-1.59368396010392,0.693086194530447));
#11916=CARTESIAN_POINT('Ctrl Pts',(3.90000423564848,-1.60111221870485,0.690188313817561));
#11917=CARTESIAN_POINT('Ctrl Pts',(3.90000407815102,-1.60816848972648,0.686450841450731));
#11918=CARTESIAN_POINT('Ctrl Pts',(3.9000032813392,-1.6147063365644,0.681954558458482));
#11919=CARTESIAN_POINT('Ctrl Pts',(3.90000284137901,-1.61831621321653,0.679471932695374));
#11920=CARTESIAN_POINT('Ctrl Pts',(3.90000222202081,-1.62176776859012,0.67675708350434));
#11921=CARTESIAN_POINT('Ctrl Pts',(3.9000016760669,-1.6250323621476,0.673818036286869));
#11922=CARTESIAN_POINT('Ctrl Pts',(3.90000114791654,-1.62819049732732,0.670974831382826));
#11923=CARTESIAN_POINT('Ctrl Pts',(3.90000068451114,-1.63115458712464,0.667938911589952));
#11924=CARTESIAN_POINT('Ctrl Pts',(3.90000068976928,-1.6339023205034,0.664721489040691));
#11925=CARTESIAN_POINT('Ctrl Pts',(3.90000069956116,-1.63901923218135,0.658729908073458));
#11926=CARTESIAN_POINT('Ctrl Pts',(3.9000021571807,-1.64338878348726,0.652110283780478));
#11927=CARTESIAN_POINT('Ctrl Pts',(3.90000267296827,-1.64695081636755,0.645027851744832));
#11928=CARTESIAN_POINT('Ctrl Pts',(3.90000272641596,-1.64731992654249,0.644293945625623));
#11929=CARTESIAN_POINT('Ctrl Pts',(3.90000277224081,-1.64768032438231,0.643555049900053));
#11930=CARTESIAN_POINT('Ctrl Pts',(3.90000280957334,-1.64803191324525,0.642811337026806));
#11931=CARTESIAN_POINT('Ctrl Pts',(3.90000316967295,-1.65142324611312,0.635637680016741));
#11932=CARTESIAN_POINT('Ctrl Pts',(3.90000247513984,-1.65395957542788,0.628100801230905));
#11933=CARTESIAN_POINT('Ctrl Pts',(3.90000142932204,-1.65558732484325,0.62036898832433));
#11934=CARTESIAN_POINT('Ctrl Pts',(3.90000076044003,-1.65662839749185,0.615423891207338));
#11935=CARTESIAN_POINT('Ctrl Pts',(3.9,-1.65729694754734,0.61039839235075));
#11936=CARTESIAN_POINT('Ctrl Pts',(3.9,-1.657567947596,0.605334330700044));
#11937=CARTESIAN_POINT('',(3.9,1.55753217754922,0.7));
#11938=CARTESIAN_POINT('',(3.9,0.883148148148148,0.7));
#11939=CARTESIAN_POINT('',(3.9,1.657567947596,0.605334330700044));
#11940=CARTESIAN_POINT('Ctrl Pts',(3.9,1.657567947596,0.605334330700044));
#11941=CARTESIAN_POINT('Ctrl Pts',(3.9,1.65714453107083,0.613246533660879));
#11942=CARTESIAN_POINT('Ctrl Pts',(3.90000169450566,1.65575314729854,0.621067109624563));
#11943=CARTESIAN_POINT('Ctrl Pts',(3.900002426785,1.653477907766,0.628635640467799));
#11944=CARTESIAN_POINT('Ctrl Pts',(3.90000283370343,1.65221358571927,0.632841378048222));
#11945=CARTESIAN_POINT('Ctrl Pts',(3.90000300372053,1.65067534627202,0.636969322077829));
#11946=CARTESIAN_POINT('Ctrl Pts',(3.90000288278183,1.6488710006323,0.640990000951852));
#11947=CARTESIAN_POINT('Ctrl Pts',(3.90000266510116,1.6456233127241,0.64822692378658));
#11948=CARTESIAN_POINT('Ctrl Pts',(3.90000136145047,1.64155197609259,0.655037842274187));
#11949=CARTESIAN_POINT('Ctrl Pts',(3.9000008487987,1.63672139510901,0.661259788874982));
#11950=CARTESIAN_POINT('Ctrl Pts',(3.90000075195303,1.63580884415802,0.662435184403355));
#11951=CARTESIAN_POINT('Ctrl Pts',(3.90000069125178,1.63486906637168,0.663589490553999));
#11952=CARTESIAN_POINT('Ctrl Pts',(3.90000068992127,1.63390232051248,0.664721489040685));
#11953=CARTESIAN_POINT('Ctrl Pts',(3.90000068733544,1.63202347103487,0.666921503393101));
#11954=CARTESIAN_POINT('Ctrl Pts',(3.9000009071255,1.6300427915863,0.669037305429552));
#11955=CARTESIAN_POINT('Ctrl Pts',(3.90000121037842,1.62796736695056,0.671065303566633));
#11956=CARTESIAN_POINT('Ctrl Pts',(3.90000204102081,1.62228255539437,0.676620208836154));
#11957=CARTESIAN_POINT('Ctrl Pts',(3.90000335328325,1.61595386407616,0.681456575151491));
#11958=CARTESIAN_POINT('Ctrl Pts',(3.90000380482706,1.60914557515952,0.685520902406533));
#11959=CARTESIAN_POINT('Ctrl Pts',(3.90000409284089,1.60480295930069,0.688113302965514));
#11960=CARTESIAN_POINT('Ctrl Pts',(3.90000408819389,1.6002642541482,0.690390927291682));
#11961=CARTESIAN_POINT('Ctrl Pts',(3.90000378365133,1.59556629223371,0.692330537597694));
#11962=CARTESIAN_POINT('Ctrl Pts',(3.90000330864444,1.58823869807682,0.695355823328757));
#11963=CARTESIAN_POINT('Ctrl Pts',(3.90000209726118,1.58060840086481,0.697526456028474));
#11964=CARTESIAN_POINT('Ctrl Pts',(3.90000112250675,1.5728228815436,0.698773197673241));
#11965=CARTESIAN_POINT('Ctrl Pts',(3.90000049100668,1.56777898966077,0.699580906164169));
#11966=CARTESIAN_POINT('Ctrl Pts',(3.89999999374416,1.56266934880282,0.69999999924861));
#11967=CARTESIAN_POINT('Ctrl Pts',(3.89999999700315,1.55753217437,0.7));
#11968=CARTESIAN_POINT('Ctrl Pts',(3.9,1.68995649764597,0.));
#11969=CARTESIAN_POINT('Ctrl Pts',(3.9,1.68454744095908,0.101111134163871));
#11970=CARTESIAN_POINT('Ctrl Pts',(3.9,1.67913787721413,0.202223216861756));
#11971=CARTESIAN_POINT('Ctrl Pts',(3.9,1.66834172806373,0.404000675610066));
#11972=CARTESIAN_POINT('Ctrl Pts',(3.9,1.66295504272671,0.504667995047933));
#11973=CARTESIAN_POINT('Ctrl Pts',(3.9,1.657567947596,0.605334330700044));
#11974=CARTESIAN_POINT('Ctrl Pts',(3.90000000000029,-1.68995649764598,2.25514051876985E-17));
#11975=CARTESIAN_POINT('Ctrl Pts',(3.90375240214247,-1.67935614215062,0.202290156525516));
#11976=CARTESIAN_POINT('Ctrl Pts',(3.90750491350916,-1.66875579641967,0.404580311547879));
#11977=CARTESIAN_POINT('Ctrl Pts',(3.91125753584366,-1.65815546066147,0.606870465045848));
#11978=CARTESIAN_POINT('Ctrl Pts',(2.95719731373254,-1.63434162994996,-0.000186284957671625));
#11979=CARTESIAN_POINT('Ctrl Pts',(2.96263618266967,-1.62374249289717,0.202103577800055));
#11980=CARTESIAN_POINT('Ctrl Pts',(2.96807524459186,-1.6131433886527,0.404393433349269));
#11981=CARTESIAN_POINT('Ctrl Pts',(2.97351444051957,-1.60254429060724,0.606683290324339));
#11982=CARTESIAN_POINT('Ctrl Pts',(2.0151035222252,-1.5373601393942,-0.000515615972119944));
#11983=CARTESIAN_POINT('Ctrl Pts',(2.0222299762717,-1.52676329064944,0.20177372753372));
#11984=CARTESIAN_POINT('Ctrl Pts',(2.02935668076532,-1.51616649670304,0.404063061036967));
#11985=CARTESIAN_POINT('Ctrl Pts',(2.03648357820815,-1.50556972342972,0.606352393906678));
#11986=CARTESIAN_POINT('Ctrl Pts',(1.07355614839761,-1.3885225322474,-0.00102014041634142));
#11987=CARTESIAN_POINT('Ctrl Pts',(1.08237048982668,-1.37792954541675,0.201268457136957));
#11988=CARTESIAN_POINT('Ctrl Pts',(1.09118510562603,-1.36733662501784,0.403557046289628));
#11989=CARTESIAN_POINT('Ctrl Pts',(1.09999999998551,-1.35674377243019,0.605845626932519));
#11990=CARTESIAN_POINT('Ctrl Pts',(1.10000000359112,-1.35674374984279,0.605845627045242));
#11991=CARTESIAN_POINT('Ctrl Pts',(2.02777573897866,-1.50422778688462,0.60559460123127));
#11992=CARTESIAN_POINT('Ctrl Pts',(2.96295221054883,-1.60165319397541,0.605428415101273));
#11993=CARTESIAN_POINT('Ctrl Pts',(3.9,-1.657567947596,0.605334330700044));
#11994=CARTESIAN_POINT('Ctrl Pts',(3.90594750914669,-1.55788759822396,0.7));
#11995=CARTESIAN_POINT('Ctrl Pts',(2.96654482017732,-1.50183737247472,0.7));
#11996=CARTESIAN_POINT('Ctrl Pts',(2.02939151553635,-1.40396309164617,0.7));
#11997=CARTESIAN_POINT('Ctrl Pts',(1.1,-1.25565664448621,0.7));
#11998=CARTESIAN_POINT('Ctrl Pts',(3.90422602671531,-1.58673967158186,0.7));
#11999=CARTESIAN_POINT('Ctrl Pts',(2.9639697519154,-1.53062009474021,0.699999324449154));
#12000=CARTESIAN_POINT('Ctrl Pts',(2.02587169016863,-1.43262076012027,0.700001792708215));
#12001=CARTESIAN_POINT('Ctrl Pts',(1.09546090287069,-1.28410178925883,0.700000000000001));
#12002=CARTESIAN_POINT('Ctrl Pts',(3.90124198563808,-1.6367522482393,0.676652244116846));
#12003=CARTESIAN_POINT('Ctrl Pts',(2.95951584878018,-1.58051528054544,0.676683243227538));
#12004=CARTESIAN_POINT('Ctrl Pts',(2.01975879699698,-1.48229505764113,0.676737195552829));
#12005=CARTESIAN_POINT('Ctrl Pts',(1.08759175402576,-1.33341535796084,0.676819902351873));
#12006=CARTESIAN_POINT('Ctrl Pts',(3.90006887217438,-1.65641364884095,0.626981005337021));
#12007=CARTESIAN_POINT('Ctrl Pts',(2.95775794493813,-1.6001648299169,0.627061170854983));
#12008=CARTESIAN_POINT('Ctrl Pts',(2.01735267249256,-1.50192280897576,0.627202240820629));
#12009=CARTESIAN_POINT('Ctrl Pts',(1.08446813262788,-1.35299014570964,0.627416665943555));
#12010=CARTESIAN_POINT('Ctrl Pts',(3.9,-1.657567947596,0.605334330700044));
#12011=CARTESIAN_POINT('Ctrl Pts',(2.95765589353472,-1.60133715645388,0.605428946878649));
#12012=CARTESIAN_POINT('Ctrl Pts',(2.01720431860088,-1.50312513840151,0.605596482146283));
#12013=CARTESIAN_POINT('Ctrl Pts',(1.0842689834292,-1.35423815332579,0.605849891671036));
#12014=CARTESIAN_POINT('Ctrl Pts',(3.89999999700313,-1.55753217437,0.7));
#12015=CARTESIAN_POINT('Ctrl Pts',(2.96258932077475,-1.50142404037792,0.7));
#12016=CARTESIAN_POINT('Ctrl Pts',(2.02743012901897,-1.40365010593343,0.7));
#12017=CARTESIAN_POINT('Ctrl Pts',(1.1,-1.25565664448621,0.7));
#12018=CARTESIAN_POINT('Origin',(6.08012166120517,1.06778195214465E-16,
0.7));
#12019=CARTESIAN_POINT('Ctrl Pts',(1.1,1.25565664448621,0.7));
#12020=CARTESIAN_POINT('Ctrl Pts',(2.02743012901899,1.40365010593344,0.7));
#12021=CARTESIAN_POINT('Ctrl Pts',(2.96258932077472,1.50142404037792,0.7));
#12022=CARTESIAN_POINT('Ctrl Pts',(3.89999999700315,1.55753217437,0.7));
#12023=CARTESIAN_POINT('Ctrl Pts',(1.1,1.25565664448621,0.7));
#12024=CARTESIAN_POINT('Ctrl Pts',(2.02939151553637,1.40396309164617,0.7));
#12025=CARTESIAN_POINT('Ctrl Pts',(2.96654482017727,1.50183737247472,0.7));
#12026=CARTESIAN_POINT('Ctrl Pts',(3.90594750914669,1.55788759822396,0.7));
#12027=CARTESIAN_POINT('Ctrl Pts',(1.09546090287069,1.28410178925883,0.700000000000001));
#12028=CARTESIAN_POINT('Ctrl Pts',(2.02587169016866,1.43262076012027,0.700001792708215));
#12029=CARTESIAN_POINT('Ctrl Pts',(2.96396975191535,1.53062009474021,0.699999324449154));
#12030=CARTESIAN_POINT('Ctrl Pts',(3.90422602671531,1.58673967158186,0.7));
#12031=CARTESIAN_POINT('Ctrl Pts',(1.08759175402576,1.33341535796084,0.676819902351873));
#12032=CARTESIAN_POINT('Ctrl Pts',(2.019758796997,1.48229505764113,0.676737195552829));
#12033=CARTESIAN_POINT('Ctrl Pts',(2.95951584878014,1.58051528054544,0.676683243227538));
#12034=CARTESIAN_POINT('Ctrl Pts',(3.90124198563808,1.6367522482393,0.676652244116846));
#12035=CARTESIAN_POINT('Ctrl Pts',(1.08446813262788,1.35299014570964,0.627416665943555));
#12036=CARTESIAN_POINT('Ctrl Pts',(2.01735267249258,1.50192280897576,0.627202240820629));
#12037=CARTESIAN_POINT('Ctrl Pts',(2.95775794493809,1.6001648299169,0.627061170854983));
#12038=CARTESIAN_POINT('Ctrl Pts',(3.90006887217438,1.65641364884095,0.626981005337021));
#12039=CARTESIAN_POINT('Ctrl Pts',(1.0842689834292,1.35423815332579,0.605849891671036));
#12040=CARTESIAN_POINT('Ctrl Pts',(2.0172043186009,1.50312513840152,0.605596482146283));
#12041=CARTESIAN_POINT('Ctrl Pts',(2.95765589353468,1.60133715645387,0.605428946878649));
#12042=CARTESIAN_POINT('Ctrl Pts',(3.9,1.657567947596,0.605334330700044));
#12043=CARTESIAN_POINT('Ctrl Pts',(3.9,1.657567947596,0.605334330700044));
#12044=CARTESIAN_POINT('Ctrl Pts',(2.96295221054879,1.60165319397541,0.605428415101273));
#12045=CARTESIAN_POINT('Ctrl Pts',(2.02777573897867,1.50422778688462,0.60559460123127));
#12046=CARTESIAN_POINT('Ctrl Pts',(1.10000000359111,1.35674374984279,0.605845627045242));
#12047=CARTESIAN_POINT('Ctrl Pts',(1.07355614839761,1.3885225322474,-0.00102014041634139));
#12048=CARTESIAN_POINT('Ctrl Pts',(1.08237048982668,1.37792954541676,0.201268457136957));
#12049=CARTESIAN_POINT('Ctrl Pts',(1.09118510562602,1.36733662501784,0.403557046289628));
#12050=CARTESIAN_POINT('Ctrl Pts',(1.09999999998551,1.35674377243019,0.605845626932519));
#12051=CARTESIAN_POINT('Ctrl Pts',(2.0151035222252,1.5373601393942,-0.000515615972119942));
#12052=CARTESIAN_POINT('Ctrl Pts',(2.0222299762717,1.52676329064944,0.201773727533721));
#12053=CARTESIAN_POINT('Ctrl Pts',(2.02935668076532,1.51616649670304,0.404063061036968));
#12054=CARTESIAN_POINT('Ctrl Pts',(2.03648357820815,1.50556972342972,0.606352393906678));
#12055=CARTESIAN_POINT('Ctrl Pts',(2.95719731373254,1.63434162994996,-0.000186284957671606));
#12056=CARTESIAN_POINT('Ctrl Pts',(2.96263618266967,1.62374249289717,0.202103577800055));
#12057=CARTESIAN_POINT('Ctrl Pts',(2.96807524459186,1.6131433886527,0.404393433349269));
#12058=CARTESIAN_POINT('Ctrl Pts',(2.97351444051957,1.60254429060724,0.60668329032434));
#12059=CARTESIAN_POINT('Ctrl Pts',(3.90000000000029,1.68995649764598,4.33680868994202E-17));
#12060=CARTESIAN_POINT('Ctrl Pts',(3.90375240214247,1.67935614215062,0.202290156525516));
#12061=CARTESIAN_POINT('Ctrl Pts',(3.90750491350917,1.66875579641967,0.404580311547879));
#12062=CARTESIAN_POINT('Ctrl Pts',(3.91125753584366,1.65815546066147,0.606870465045848));
#12063=CARTESIAN_POINT('Origin',(0.9,1.44962962962963,0.));
#12064=CARTESIAN_POINT('',(0.900000000000025,-1.32415632515176,0.605901073595307));
#12065=CARTESIAN_POINT('Ctrl Pts',(0.900000000000025,-1.32415632515176,
0.605901073595307));
#12066=CARTESIAN_POINT('Ctrl Pts',(0.900000000000025,-1.33021622058432,
0.504787384877132));
#12067=CARTESIAN_POINT('Ctrl Pts',(0.900000000000001,-1.33627289299046,
0.403672458220672));
#12068=CARTESIAN_POINT('Ctrl Pts',(0.900000000000001,-1.3483639425303,0.201706128802639));
#12069=CARTESIAN_POINT('Ctrl Pts',(0.9,-1.3543984610184,0.100852646477479));
#12070=CARTESIAN_POINT('Ctrl Pts',(0.9,-1.3604297237941,0.));
#12071=CARTESIAN_POINT('',(0.9,-1.22294421121193,0.7));
#12072=CARTESIAN_POINT('Ctrl Pts',(0.899999998934589,-1.2229442093848,0.7));
#12073=CARTESIAN_POINT('Ctrl Pts',(0.89999998269596,-1.2309559991361,0.699999991698178));
#12074=CARTESIAN_POINT('Ctrl Pts',(0.900003161357076,-1.2389110096839,0.699008412490225));
#12075=CARTESIAN_POINT('Ctrl Pts',(0.900005837532895,-1.24666554379878,
0.697120920272419));
#12076=CARTESIAN_POINT('Ctrl Pts',(0.900007138246235,-1.25043451364619,
0.69620353424371));
#12077=CARTESIAN_POINT('Ctrl Pts',(0.900008321383585,-1.25415610217771,
0.695073675615989));
#12078=CARTESIAN_POINT('Ctrl Pts',(0.900009136546862,-1.25781268161099,
0.69373809091454));
#12079=CARTESIAN_POINT('Ctrl Pts',(0.90001081442992,-1.26533916477404,0.690989003700189));
#12080=CARTESIAN_POINT('Ctrl Pts',(0.900010659344479,-1.27251458345821,
0.687399440976464));
#12081=CARTESIAN_POINT('Ctrl Pts',(0.900008585023094,-1.27919110928202,
0.68304500924512));
#12082=CARTESIAN_POINT('Ctrl Pts',(0.900007251085311,-1.28348459539356,
0.680244796581297));
#12083=CARTESIAN_POINT('Ctrl Pts',(0.900005156998288,-1.28757155292352,
0.67712723751572));
#12084=CARTESIAN_POINT('Ctrl Pts',(0.900003422242992,-1.29140570811059,
0.673703384872626));
#12085=CARTESIAN_POINT('Ctrl Pts',(0.90000203719427,-1.29446694202502,0.670969741262059));
#12086=CARTESIAN_POINT('Ctrl Pts',(0.90000088611098,-1.29734878548314,0.668056850549005));
#12087=CARTESIAN_POINT('Ctrl Pts',(0.900000936626746,-1.30003070819003,
0.664973821719563));
#12088=CARTESIAN_POINT('Ctrl Pts',(0.90000103432908,-1.30521780373233,0.659010948495488));
#12089=CARTESIAN_POINT('Ctrl Pts',(0.900005119671874,-1.30966005175478,
0.652412896960716));
#12090=CARTESIAN_POINT('Ctrl Pts',(0.900006662646281,-1.31329014967729,
0.64534035177384));
#12091=CARTESIAN_POINT('Ctrl Pts',(0.900006837929091,-1.31370253096037,
0.644536906434065));
#12092=CARTESIAN_POINT('Ctrl Pts',(0.900006988901759,-1.3141043809937,0.64372731654354));
#12093=CARTESIAN_POINT('Ctrl Pts',(0.900007112770807,-1.31449556093743,
0.642911804846506));
#12094=CARTESIAN_POINT('Ctrl Pts',(0.900008198175579,-1.31792328224658,
0.635765868899185));
#12095=CARTESIAN_POINT('Ctrl Pts',(0.900006415208278,-1.32049402672979,
0.628253543462219));
#12096=CARTESIAN_POINT('Ctrl Pts',(0.900003664797616,-1.32215034643222,
0.620540220943237));
#12097=CARTESIAN_POINT('Ctrl Pts',(0.900001948338234,-1.32318401225236,
0.615726538031782));
#12098=CARTESIAN_POINT('Ctrl Pts',(0.900000000000001,-1.32386068836271,
0.610833984830158));
#12099=CARTESIAN_POINT('Ctrl Pts',(0.900000000000001,-1.32415632515176,
0.605901073595307));
#12100=CARTESIAN_POINT('',(0.9,1.22294421121193,0.7));
#12101=CARTESIAN_POINT('',(0.9,0.724814814814815,0.7));
#12102=CARTESIAN_POINT('',(0.900000000000027,1.32415632515176,0.605901073595307));
#12103=CARTESIAN_POINT('Ctrl Pts',(0.900000000000001,1.32415632515176,0.605901073595307));
#12104=CARTESIAN_POINT('Ctrl Pts',(0.900000000000001,1.32368299187747,0.613798977756921));
#12105=CARTESIAN_POINT('Ctrl Pts',(0.900004523569871,1.32223544152535,0.621596324701597));
#12106=CARTESIAN_POINT('Ctrl Pts',(0.900006356724635,1.31990036466821,0.629134362570908));
#12107=CARTESIAN_POINT('Ctrl Pts',(0.900007328861843,1.3186620540024,0.633131846706937));
#12108=CARTESIAN_POINT('Ctrl Pts',(0.900007702029268,1.31717322147439,0.637056437951431));
#12109=CARTESIAN_POINT('Ctrl Pts',(0.900007358328755,1.31544117393516,0.640882963165587));
#12110=CARTESIAN_POINT('Ctrl Pts',(0.900006707239278,1.31216006761937,0.648131745755711));
#12111=CARTESIAN_POINT('Ctrl Pts',(0.900003091243194,1.3080468004769,0.654946293188228));
#12112=CARTESIAN_POINT('Ctrl Pts',(0.900001489347898,1.30317324258861,0.661167512355852));
#12113=CARTESIAN_POINT('Ctrl Pts',(0.900001155878064,1.30215870403359,0.662462596327245));
#12114=CARTESIAN_POINT('Ctrl Pts',(0.90000093695446,1.30111105636563,0.663731893727214));
#12115=CARTESIAN_POINT('Ctrl Pts',(0.90000091848414,1.30003070515708,0.664973821721807));
#12116=CARTESIAN_POINT('Ctrl Pts',(0.90000089007412,1.29836896897911,0.666884086330845));
#12117=CARTESIAN_POINT('Ctrl Pts',(0.900001333486324,1.29662987445651,0.668729618924651));
#12118=CARTESIAN_POINT('Ctrl Pts',(0.900001997973453,1.2948182721625,0.670508241825176));
#12119=CARTESIAN_POINT('Ctrl Pts',(0.900004083621534,1.28913213515815,0.676090865298813));
#12120=CARTESIAN_POINT('Ctrl Pts',(0.900007925915178,1.28279871831387,0.680954424681199));
#12121=CARTESIAN_POINT('Ctrl Pts',(0.900009431597099,1.27598654051802,0.685053039288488));
#12122=CARTESIAN_POINT('Ctrl Pts',(0.900010426918848,1.2714833923965,0.687762403198649));
#12123=CARTESIAN_POINT('Ctrl Pts',(0.900010579450444,1.26676996242859,0.690136867340003));
#12124=CARTESIAN_POINT('Ctrl Pts',(0.900009885932263,1.26188774903006,0.692153145632694));
#12125=CARTESIAN_POINT('Ctrl Pts',(0.900008832351734,1.25447077696631,0.695216239878874));
#12126=CARTESIAN_POINT('Ctrl Pts',(0.900005746465811,1.24674633448708,0.697421320974322));
#12127=CARTESIAN_POINT('Ctrl Pts',(0.900003140090462,1.23886595492982,0.6987028844583));
#12128=CARTESIAN_POINT('Ctrl Pts',(0.900001403206082,1.23361448254879,0.699556916322089));
#12129=CARTESIAN_POINT('Ctrl Pts',(0.899999988093253,1.22829309040712,0.699999994457486));
#12130=CARTESIAN_POINT('Ctrl Pts',(0.899999998934588,1.2229442093848,0.7));
#12131=CARTESIAN_POINT('Ctrl Pts',(0.9,1.3604297237941,0.));
#12132=CARTESIAN_POINT('Ctrl Pts',(0.9,1.35439838926384,0.100853846331769));
#12133=CARTESIAN_POINT('Ctrl Pts',(0.9,1.34836379894337,0.201708528537181));
#12134=CARTESIAN_POINT('Ctrl Pts',(0.9,1.33627274925098,0.403674857922336));
#12135=CARTESIAN_POINT('Ctrl Pts',(0.900000000000027,1.33021614867672,0.504788584706939));
#12136=CARTESIAN_POINT('Ctrl Pts',(0.900000000000027,1.32415632515176,0.605901073595307));
#12137=CARTESIAN_POINT('Ctrl Pts',(0.900000000000001,-1.3604297237941,-1.73472347597681E-18));
#12138=CARTESIAN_POINT('Ctrl Pts',(0.909119345746934,-1.34984469470005,
0.202150401646216));
#12139=CARTESIAN_POINT('Ctrl Pts',(0.918238975454288,-1.33925973741039,
0.404300794324169));
#12140=CARTESIAN_POINT('Ctrl Pts',(0.92735889343571,-1.32867485341111,0.606451177918334));
#12141=CARTESIAN_POINT('Ctrl Pts',(0.693791632045388,-1.32642527651154,
-0.000115194085079675));
#12142=CARTESIAN_POINT('Ctrl Pts',(0.703280422539661,-1.31584113310577,
0.202035038813999));
#12143=CARTESIAN_POINT('Ctrl Pts',(0.712769508818954,-1.30525706820637,
0.404185262036053));
#12144=CARTESIAN_POINT('Ctrl Pts',(0.722258895242942,-1.29467308328318,
0.606335475483814));
#12145=CARTESIAN_POINT('Ctrl Pts',(0.487608314405001,-1.28990207050556,
-0.000238777108575344));
#12146=CARTESIAN_POINT('Ctrl Pts',(0.497466558273561,-1.27931888757273,
0.201911276725417));
#12147=CARTESIAN_POINT('Ctrl Pts',(0.507325109482935,-1.26873579028159,
0.404061320158324));
#12148=CARTESIAN_POINT('Ctrl Pts',(0.517183972542757,-1.25815278023897,
0.606211353085106));
#12149=CARTESIAN_POINT('Ctrl Pts',(0.281447431601629,-1.2507496025167,-0.000370926150909055));
#12150=CARTESIAN_POINT('Ctrl Pts',(0.291675125201343,-1.24016745708839,
0.201778938960696));
#12151=CARTESIAN_POINT('Ctrl Pts',(0.301903137322998,-1.2295854048496,0.403928792940867));
#12152=CARTESIAN_POINT('Ctrl Pts',(0.312131472716966,-1.21900344770756,
0.606078635650713));
#12153=CARTESIAN_POINT('',(0.313137632044026,-1.21919552599285,0.606079286803921));
#12154=CARTESIAN_POINT('Ctrl Pts',(0.28146619846596,-1.25073018526678,-6.36968776335234E-17));
#12155=CARTESIAN_POINT('Ctrl Pts',(0.292023490345879,-1.2402182973453,0.20202640462578));
#12156=CARTESIAN_POINT('Ctrl Pts',(0.302580635585432,-1.22970674279184,
0.404052833452346));
#12157=CARTESIAN_POINT('Ctrl Pts',(0.313137632044028,-1.21919552599286,
0.606079286803922));
#12158=CARTESIAN_POINT('Ctrl Pts',(0.313137632044026,-1.21919552599285,
0.606079286803921));
#12159=CARTESIAN_POINT('Ctrl Pts',(0.508347756773358,-1.25646926692181,
0.606016122348466));
#12160=CARTESIAN_POINT('Ctrl Pts',(0.703992099548353,-1.29143758865737,
0.605956720831638));
#12161=CARTESIAN_POINT('Ctrl Pts',(0.900000000000031,-1.32415632515176,
0.605901073595307));
#12162=CARTESIAN_POINT('Ctrl Pts',(0.916434425702686,-1.22569269236154,
0.7));
#12163=CARTESIAN_POINT('Ctrl Pts',(0.72117838049967,-1.193102781986,0.7));
#12164=CARTESIAN_POINT('Ctrl Pts',(0.526295996270969,-1.15827411715321,
0.7));
#12165=CARTESIAN_POINT('Ctrl Pts',(0.3318563713692,-1.12115139781564,0.7));
#12166=CARTESIAN_POINT('Ctrl Pts',(0.911693828447622,-1.25409504944868,
0.700000000000001));
#12167=CARTESIAN_POINT('Ctrl Pts',(0.716221724293519,-1.22145811194286,
0.699999606692487));
#12168=CARTESIAN_POINT('Ctrl Pts',(0.52112301919326,-1.18657973614434,0.700000445015345));
#12169=CARTESIAN_POINT('Ctrl Pts',(0.32646265058614,-1.14940237362229,0.699999999999999));
#12170=CARTESIAN_POINT('Ctrl Pts',(0.903473253113197,-1.30334701150065,
0.676847307332805));
#12171=CARTESIAN_POINT('Ctrl Pts',(0.707628846166824,-1.27063023858114,
0.676865462359186));
#12172=CARTESIAN_POINT('Ctrl Pts',(0.512149925983835,-1.23566412474798,
0.676884474751893));
#12173=CARTESIAN_POINT('Ctrl Pts',(0.317109102097966,-1.19839394783867,
0.676905055067496));
#12174=CARTESIAN_POINT('Ctrl Pts',(0.900209809599689,-1.32289929215588,
0.627459885485154));
#12175=CARTESIAN_POINT('Ctrl Pts',(0.704212910592823,-1.29017057588713,
0.627506965865002));
#12176=CARTESIAN_POINT('Ctrl Pts',(0.50858160780484,-1.25519230329596,0.627556915196293));
#12177=CARTESIAN_POINT('Ctrl Pts',(0.31338355686088,-1.21790743260971,0.627610331402299));
#12178=CARTESIAN_POINT('Ctrl Pts',(0.900000000000031,-1.32415632515176,
0.605901073595307));
#12179=CARTESIAN_POINT('Ctrl Pts',(0.703992099548353,-1.29143758865737,
0.605956720831638));
#12180=CARTESIAN_POINT('Ctrl Pts',(0.508347756773358,-1.25646926692181,
0.606016122348466));
#12181=CARTESIAN_POINT('Ctrl Pts',(0.313137632044026,-1.21919552599285,
0.606079286803921));
#12182=CARTESIAN_POINT('',(0.3318563713692,-1.12115139781563,0.7));
#12183=CARTESIAN_POINT('Origin',(0.331856371369202,-1.12115139781563,0.6));
#12184=CARTESIAN_POINT('Ctrl Pts',(0.899999998934586,-1.2229442093848,0.7));
#12185=CARTESIAN_POINT('Ctrl Pts',(0.71024282334811,-1.19114655107378,0.7));
#12186=CARTESIAN_POINT('Ctrl Pts',(0.520840466228891,-1.15723253876768,
0.7));
#12187=CARTESIAN_POINT('Ctrl Pts',(0.3318563713692,-1.12115139781564,0.7));
#12188=CARTESIAN_POINT('Origin',(6.08012166120517,1.06778195214465E-16,
0.7));
#12189=CARTESIAN_POINT('',(0.331856371369203,1.12115139781563,0.7));
#12190=CARTESIAN_POINT('',(0.3318563713692,-0.7,0.7));
#12191=CARTESIAN_POINT('Ctrl Pts',(0.331856371369202,1.12115139781564,0.7));
#12192=CARTESIAN_POINT('Ctrl Pts',(0.520840466228894,1.15723253876768,0.7));
#12193=CARTESIAN_POINT('Ctrl Pts',(0.710242823348114,1.19114655107378,0.7));
#12194=CARTESIAN_POINT('Ctrl Pts',(0.899999998934589,1.2229442093848,0.7));
#12195=CARTESIAN_POINT('Ctrl Pts',(0.281447431601628,1.2507496025167,-0.000370926150909064));
#12196=CARTESIAN_POINT('Ctrl Pts',(0.291675125201342,1.24016745708839,0.201778938960695));
#12197=CARTESIAN_POINT('Ctrl Pts',(0.301903137322998,1.2295854048496,0.403928792940867));
#12198=CARTESIAN_POINT('Ctrl Pts',(0.312131472716965,1.21900344770756,0.606078635650713));
#12199=CARTESIAN_POINT('Ctrl Pts',(0.487608314405001,1.28990207050556,-0.000238777108575355));
#12200=CARTESIAN_POINT('Ctrl Pts',(0.497466558273561,1.27931888757273,0.201911276725417));
#12201=CARTESIAN_POINT('Ctrl Pts',(0.507325109482935,1.26873579028159,0.404061320158324));
#12202=CARTESIAN_POINT('Ctrl Pts',(0.517183972542757,1.25815278023897,0.606211353085106));
#12203=CARTESIAN_POINT('Ctrl Pts',(0.693791632045388,1.32642527651154,-0.000115194085079627));
#12204=CARTESIAN_POINT('Ctrl Pts',(0.703280422539661,1.31584113310577,0.202035038813999));
#12205=CARTESIAN_POINT('Ctrl Pts',(0.712769508818955,1.30525706820637,0.404185262036054));
#12206=CARTESIAN_POINT('Ctrl Pts',(0.722258895242942,1.29467308328318,0.606335475483814));
#12207=CARTESIAN_POINT('Ctrl Pts',(0.900000000000002,1.3604297237941,4.33680868994202E-17));
#12208=CARTESIAN_POINT('Ctrl Pts',(0.909119345746935,1.34984469470005,0.202150401646216));
#12209=CARTESIAN_POINT('Ctrl Pts',(0.918238975454289,1.33925973741039,0.40430079432417));
#12210=CARTESIAN_POINT('Ctrl Pts',(0.927358893435711,1.32867485341111,0.606451177918334));
#12211=CARTESIAN_POINT('',(0.313137632044028,1.21919552599286,0.606079286803921));
#12212=CARTESIAN_POINT('Ctrl Pts',(0.900000000000026,1.32415632515176,0.605901073595307));
#12213=CARTESIAN_POINT('Ctrl Pts',(0.703992099548352,1.29143758865737,0.605956720831638));
#12214=CARTESIAN_POINT('Ctrl Pts',(0.508347756773358,1.25646926692181,0.606016122348466));
#12215=CARTESIAN_POINT('Ctrl Pts',(0.313137632044028,1.21919552599286,0.606079286803921));
#12216=CARTESIAN_POINT('Ctrl Pts',(0.313137632044028,1.21919552599286,0.606079286803922));
#12217=CARTESIAN_POINT('Ctrl Pts',(0.302580635585432,1.22970674279184,0.404052833452346));
#12218=CARTESIAN_POINT('Ctrl Pts',(0.29202349034588,1.2402182973453,0.20202640462578));
#12219=CARTESIAN_POINT('Ctrl Pts',(0.28146619846596,1.25073018526678,-6.5594231435373E-18));
#12220=CARTESIAN_POINT('Ctrl Pts',(0.331856371369202,1.12115139781564,0.7));
#12221=CARTESIAN_POINT('Ctrl Pts',(0.526295996270969,1.15827411715321,0.7));
#12222=CARTESIAN_POINT('Ctrl Pts',(0.72117838049967,1.193102781986,0.7));
#12223=CARTESIAN_POINT('Ctrl Pts',(0.916434425702682,1.22569269236154,0.7));
#12224=CARTESIAN_POINT('Ctrl Pts',(0.326462650586141,1.14940237362229,0.699999999999999));
#12225=CARTESIAN_POINT('Ctrl Pts',(0.52112301919326,1.18657973614434,0.700000445015345));
#12226=CARTESIAN_POINT('Ctrl Pts',(0.716221724293519,1.22145811194286,0.699999606692487));
#12227=CARTESIAN_POINT('Ctrl Pts',(0.911693828447618,1.25409504944868,0.700000000000001));
#12228=CARTESIAN_POINT('Ctrl Pts',(0.317109102097967,1.19839394783867,0.676905055067496));
#12229=CARTESIAN_POINT('Ctrl Pts',(0.512149925983836,1.23566412474798,0.676884474751893));
#12230=CARTESIAN_POINT('Ctrl Pts',(0.707628846166824,1.27063023858114,0.676865462359185));
#12231=CARTESIAN_POINT('Ctrl Pts',(0.903473253113193,1.30334701150065,0.676847307332805));
#12232=CARTESIAN_POINT('Ctrl Pts',(0.313383556860882,1.21790743260971,0.627610331402299));
#12233=CARTESIAN_POINT('Ctrl Pts',(0.508581607804839,1.25519230329596,0.627556915196293));
#12234=CARTESIAN_POINT('Ctrl Pts',(0.704212910592822,1.29017057588713,0.627506965865002));
#12235=CARTESIAN_POINT('Ctrl Pts',(0.900209809599685,1.32289929215587,0.627459885485154));
#12236=CARTESIAN_POINT('Ctrl Pts',(0.313137632044028,1.21919552599286,0.606079286803921));
#12237=CARTESIAN_POINT('Ctrl Pts',(0.508347756773358,1.25646926692181,0.606016122348466));
#12238=CARTESIAN_POINT('Ctrl Pts',(0.703992099548352,1.29143758865737,0.605956720831638));
#12239=CARTESIAN_POINT('Ctrl Pts',(0.900000000000026,1.32415632515176,0.605901073595307));
#12240=CARTESIAN_POINT('Origin',(0.3318563713692,1.12115139781563,0.6));
#12241=CARTESIAN_POINT('Origin',(0.3318563713692,1.12115139781563,0.6));
#12242=CARTESIAN_POINT('Origin',(0.3318563713692,1.12115139781563,0.6));
#12243=CARTESIAN_POINT('Origin',(0.331856371369201,1.12115139781563,0.6));
#12244=CARTESIAN_POINT('Origin',(11.6681436286308,1.2964346619681,0.6));
#12245=CARTESIAN_POINT('Origin',(11.6681436286308,1.2964346619681,0.6));
#12246=CARTESIAN_POINT('',(11.7680065821063,1.2964346619681,0.605233595624295));
#12247=CARTESIAN_POINT('Origin',(11.6681436286308,1.2964346619681,0.6));
#12248=CARTESIAN_POINT('Origin',(11.6681436286308,1.2964346619681,0.6));
#12249=CARTESIAN_POINT('Origin',(0.3318563713692,-1.12115139781563,0.6));
#12250=CARTESIAN_POINT('Origin',(0.3318563713692,-1.12115139781563,0.6));
#12251=CARTESIAN_POINT('Origin',(0.3318563713692,-1.12115139781563,0.6));
#12252=CARTESIAN_POINT('Origin',(0.3318563713692,-0.7,0.6));
#12253=CARTESIAN_POINT('Ctrl Pts',(0.281398851089427,-1.25079724300364,
-0.00128877254616805));
#12254=CARTESIAN_POINT('Ctrl Pts',(0.291978592719145,-1.24026300108396,
0.201167222825305));
#12255=CARTESIAN_POINT('Ctrl Pts',(0.302558187088771,-1.2297290939422,0.403623242499903));
#12256=CARTESIAN_POINT('Ctrl Pts',(0.313137632044028,-1.21919552599286,
0.606079286803922));
#12257=CARTESIAN_POINT('Ctrl Pts',(0.258825925396095,-1.24645021448495,
-0.000331836826913007));
#12258=CARTESIAN_POINT('Ctrl Pts',(0.269412087408768,-1.23590982471973,
0.202123507634926));
#12259=CARTESIAN_POINT('Ctrl Pts',(0.279998097240749,-1.22537010804418,
0.404578894752494));
#12260=CARTESIAN_POINT('Ctrl Pts',(0.290584031570127,-1.21483034200885,
0.60703428203898));
#12261=CARTESIAN_POINT('Ctrl Pts',(0.216858515231733,-1.22156435206688,
0.000573427186746937));
#12262=CARTESIAN_POINT('Ctrl Pts',(0.22746089442761,-1.21102065820065,0.20302778119957));
#12263=CARTESIAN_POINT('Ctrl Pts',(0.238063405890532,-1.20047706879609,
0.405482132943502));
#12264=CARTESIAN_POINT('Ctrl Pts',(0.248665715176951,-1.18993398276804,
0.607936521147589));
#12265=CARTESIAN_POINT('Ctrl Pts',(0.20022524016831,-1.1757120364715,-0.000939345874739115));
#12266=CARTESIAN_POINT('Ctrl Pts',(0.210835545796271,-1.16517845930889,
0.201515175954065));
#12267=CARTESIAN_POINT('Ctrl Pts',(0.221445511453644,-1.15464532122135,
0.403969738345816));
#12268=CARTESIAN_POINT('Ctrl Pts',(0.232055819885544,-1.1441124535127,0.606424296559432));
#12269=CARTESIAN_POINT('Ctrl Pts',(0.200162791320387,-1.15273540576203,
-0.00213094087794781));
#12270=CARTESIAN_POINT('Ctrl Pts',(0.210772999146098,-1.14220702337553,
0.200323884929633));
#12271=CARTESIAN_POINT('Ctrl Pts',(0.221383207999129,-1.13167901896849,
0.402778730339676));
#12272=CARTESIAN_POINT('Ctrl Pts',(0.231993417893744,-1.12115139781563,
0.605233595624295));
#12273=CARTESIAN_POINT('Origin',(11.6681436286308,-1.2964346619681,0.6));
#12274=CARTESIAN_POINT('',(11.7680065821063,-1.2964346619681,0.605233595624295));
#12275=CARTESIAN_POINT('Origin',(11.6681436286308,-1.2964346619681,0.6));
#12276=CARTESIAN_POINT('Origin',(11.6681436286308,-1.2964346619681,0.6));
#12277=CARTESIAN_POINT('Origin',(11.6681436286308,0.8,0.6));
#12278=CARTESIAN_POINT('',(11.7680065821063,0.8,0.605233595624295));
#12279=CARTESIAN_POINT('Ctrl Pts',(11.7998406965532,-1.32812796269332,-0.00219749346969486));
#12280=CARTESIAN_POINT('Ctrl Pts',(11.7892293257052,-1.31756329650235,0.200279524124498));
#12281=CARTESIAN_POINT('Ctrl Pts',(11.778617954226,-1.30699886176745,0.402756553762325));
#12282=CARTESIAN_POINT('Ctrl Pts',(11.7680065821063,-1.2964346619681,0.605233595624295));
#12283=CARTESIAN_POINT('Ctrl Pts',(11.7997644051931,-1.35610429277321,-0.000741767599518841));
#12284=CARTESIAN_POINT('Ctrl Pts',(11.7891529352516,-1.34553639595159,0.201735054786578));
#12285=CARTESIAN_POINT('Ctrl Pts',(11.7785417923834,-1.33496887357233,0.404211913913734));
#12286=CARTESIAN_POINT('Ctrl Pts',(11.7679303202531,-1.32440140973518,0.606688758469115));
#12287=CARTESIAN_POINT('Ctrl Pts',(11.777798894316,-1.40464673224301,0.000639873095493681));
#12288=CARTESIAN_POINT('Ctrl Pts',(11.7671928076068,-1.39407357725403,0.203116666245104));
#12289=CARTESIAN_POINT('Ctrl Pts',(11.7565866683578,-1.38350056680667,0.405593463707878));
#12290=CARTESIAN_POINT('Ctrl Pts',(11.7459806329718,-1.37292778989405,0.608070278434593));
#12291=CARTESIAN_POINT('Ctrl Pts',(11.7305637688674,-1.42539741767755,-0.000752904078362463));
#12292=CARTESIAN_POINT('Ctrl Pts',(11.7199663219939,-1.4148278080644,0.201724510929383));
#12293=CARTESIAN_POINT('Ctrl Pts',(11.7093688723049,-1.40425849106451,0.404201940657439));
#12294=CARTESIAN_POINT('Ctrl Pts',(11.6987715660822,-1.39368929079062,0.606679383299034));
#12295=CARTESIAN_POINT('Ctrl Pts',(11.7096810564041,-1.4274931182575,-0.0017379730583696));
#12296=CARTESIAN_POINT('Ctrl Pts',(11.6990862989954,-1.41692678914967,0.200739752511227));
#12297=CARTESIAN_POINT('Ctrl Pts',(11.6884916259906,-1.40636067879325,0.403217493356832));
#12298=CARTESIAN_POINT('Ctrl Pts',(11.6778970386953,-1.39579479040469,0.605695249702977));
#12299=CARTESIAN_POINT('Ctrl Pts',(11.7997255308004,-1.32801330383774,1.58293517182884E-17));
#12300=CARTESIAN_POINT('Ctrl Pts',(11.7891525485321,-1.31748685893698,0.201744519857947));
#12301=CARTESIAN_POINT('Ctrl Pts',(11.7785795656372,-1.30696064383315,0.403489051673192));
#12302=CARTESIAN_POINT('Ctrl Pts',(11.7680065821063,-1.2964346619681,0.605233595624295));
#12303=CARTESIAN_POINT('Ctrl Pts',(11.7096782931395,1.42749036240749,-0.00168516396645821));
#12304=CARTESIAN_POINT('Ctrl Pts',(11.6990844568337,1.41692495195436,0.200774958575157));
#12305=CARTESIAN_POINT('Ctrl Pts',(11.6884907049172,1.40635976021489,0.403235096390144));
#12306=CARTESIAN_POINT('Ctrl Pts',(11.6778970386953,1.39579479040469,0.605695249702978));
#12307=CARTESIAN_POINT('Ctrl Pts',(11.7375219088137,1.42469609383707,-0.000371738767665111));
#12308=CARTESIAN_POINT('Ctrl Pts',(11.7269244310859,1.41412622652679,0.202087962343291));
#12309=CARTESIAN_POINT('Ctrl Pts',(11.7163270893473,1.40355692684423,0.404547700208143));
#12310=CARTESIAN_POINT('Ctrl Pts',(11.7057297418778,1.39298745758592,0.607007427831054));
#12311=CARTESIAN_POINT('Ctrl Pts',(11.7837126264455,1.39812338730171,0.000662527065309348));
#12312=CARTESIAN_POINT('Ctrl Pts',(11.7731059659782,1.38755170250994,0.203121672627585));
#12313=CARTESIAN_POINT('Ctrl Pts',(11.762499302106,1.37698011891703,0.405580822779681));
#12314=CARTESIAN_POINT('Ctrl Pts',(11.7518926781287,1.36640881816393,0.608039989525598));
#12315=CARTESIAN_POINT('Ctrl Pts',(11.7997807104374,1.34910745421534,-0.00105289019631603));
#12316=CARTESIAN_POINT('Ctrl Pts',(11.7891702365097,1.33854134055748,0.201406383632416));
#12317=CARTESIAN_POINT('Ctrl Pts',(11.7785598611315,1.32797539467558,0.403865671186622));
#12318=CARTESIAN_POINT('Ctrl Pts',(11.7679493857164,1.31740972279341,0.60632496775791));
#12319=CARTESIAN_POINT('Ctrl Pts',(11.7998379289556,1.32812520727701,-0.00214468456243374));
#12320=CARTESIAN_POINT('Ctrl Pts',(11.78922748064,1.31756145959839,0.200314730064766));
#12321=CARTESIAN_POINT('Ctrl Pts',(11.7786170316934,1.30699794333589,0.402774156733522));
#12322=CARTESIAN_POINT('Ctrl Pts',(11.7680065821063,1.2964346619681,0.605233595624295));
#12323=CARTESIAN_POINT('Ctrl Pts',(11.7680065821063,1.2964346619681,0.605233595624295));
#12324=CARTESIAN_POINT('Ctrl Pts',(11.7785795656372,1.30696064383315,0.403489051673192));
#12325=CARTESIAN_POINT('Ctrl Pts',(11.7891525485321,1.31748685893698,0.201744519857946));
#12326=CARTESIAN_POINT('Ctrl Pts',(11.7997255308004,1.32801330383774,3.10081821330854E-17));
#12327=CARTESIAN_POINT('Ctrl Pts',(11.3905090053564,1.32332268868375,0.7));
#12328=CARTESIAN_POINT('Ctrl Pts',(11.4830653488871,1.31448403714216,0.7));
#12329=CARTESIAN_POINT('Ctrl Pts',(11.5756099286391,1.3055179747114,0.7));
#12330=CARTESIAN_POINT('Ctrl Pts',(11.6681436286308,1.2964346619681,0.7));
#12331=CARTESIAN_POINT('Ctrl Pts',(11.3932507170007,1.35203326785047,0.7));
#12332=CARTESIAN_POINT('Ctrl Pts',(11.4858332859074,1.34318985044544,0.699999917777441));
#12333=CARTESIAN_POINT('Ctrl Pts',(11.5784027531871,1.33421922733773,0.700000082825348));
#12334=CARTESIAN_POINT('Ctrl Pts',(11.6709605510772,1.32513126902304,0.7));
#12335=CARTESIAN_POINT('Ctrl Pts',(11.3980029235658,1.40179729139028,0.67675176769038));
#12336=CARTESIAN_POINT('Ctrl Pts',(11.4906306781252,1.39294591144353,0.676755553516685));
#12337=CARTESIAN_POINT('Ctrl Pts',(11.583243842395,1.38396722707511,0.676759299309383));
#12338=CARTESIAN_POINT('Ctrl Pts',(11.6758431636759,1.37487151491717,0.676763114282959));
#12339=CARTESIAN_POINT('Ctrl Pts',(11.3998836071583,1.4214913811319,0.627256563056779));
#12340=CARTESIAN_POINT('Ctrl Pts',(11.4925297866457,1.41264104586547,0.627266369072496));
#12341=CARTESIAN_POINT('Ctrl Pts',(11.5851604051362,1.40366358810601,0.627276165220861));
#12342=CARTESIAN_POINT('Ctrl Pts',(11.6777767156198,1.39456903283364,0.627286048421068));
#12343=CARTESIAN_POINT('Ctrl Pts',(11.4,1.4227102204299,0.605660349289938));
#12344=CARTESIAN_POINT('Ctrl Pts',(11.4926474653491,1.41386220753305,0.605671932550561));
#12345=CARTESIAN_POINT('Ctrl Pts',(11.585279512325,1.40488700096013,0.605683574233495));
#12346=CARTESIAN_POINT('Ctrl Pts',(11.6778970386953,1.39579479040469,0.605695249702977));
#12347=CARTESIAN_POINT('Ctrl Pts',(0.200160078391861,1.15273809776858,-0.00218270663797729));
#12348=CARTESIAN_POINT('Ctrl Pts',(0.210771190526905,1.14220881798213,0.200289374419605));
#12349=CARTESIAN_POINT('Ctrl Pts',(0.221382303689445,1.13167991623912,0.402761475082968));
#12350=CARTESIAN_POINT('Ctrl Pts',(0.231993417893744,1.12115139781563,0.605233595624295));
#12351=CARTESIAN_POINT('Ctrl Pts',(0.200222527243758,1.17571472979894,-0.000991111558954063));
#12352=CARTESIAN_POINT('Ctrl Pts',(0.210833737189325,1.165180254798,0.201480665494204));
#12353=CARTESIAN_POINT('Ctrl Pts',(0.22144460713556,1.15464621893915,0.403952483115279));
#12354=CARTESIAN_POINT('Ctrl Pts',(0.232055819885544,1.1441124535127,0.606424296559433));
#12355=CARTESIAN_POINT('Ctrl Pts',(0.216855804290742,1.22156704800519,0.000521661548984882));
#12356=CARTESIAN_POINT('Ctrl Pts',(0.22745908713481,1.21102245544698,0.202993270772045));
#12357=CARTESIAN_POINT('Ctrl Pts',(0.238062502254218,1.2004779673848,0.405464877727456));
#12358=CARTESIAN_POINT('Ctrl Pts',(0.248665715176951,1.18993398276804,0.607936521147589));
#12359=CARTESIAN_POINT('Ctrl Pts',(0.258823218619159,1.24645290953083,-0.000383602721372307));
#12360=CARTESIAN_POINT('Ctrl Pts',(0.269410282911183,1.23591162135389,0.202088997034388));
#12361=CARTESIAN_POINT('Ctrl Pts',(0.279997195000074,1.22537100634993,0.404561639451295));
#12362=CARTESIAN_POINT('Ctrl Pts',(0.290584031570127,1.21483034200885,0.60703428203898));
#12363=CARTESIAN_POINT('Ctrl Pts',(0.281396145950812,1.25079993650842,-0.00134053860524368));
#12364=CARTESIAN_POINT('Ctrl Pts',(0.291976789318506,1.24026479669674,0.201132712115111));
#12365=CARTESIAN_POINT('Ctrl Pts',(0.302557285401186,1.22972999171968,0.403605987142707));
#12366=CARTESIAN_POINT('Ctrl Pts',(0.313137632044028,1.21919552599286,0.606079286803922));
#12367=CARTESIAN_POINT('Origin',(11.8002740930491,1.6,-0.0104671912485888));
#12368=CARTESIAN_POINT('Origin',(0.3318563713692,1.12115139781563,0.6));
#12369=CARTESIAN_POINT('',(0.331856371369203,1.12115139781563,0.9));
#12370=CARTESIAN_POINT('',(0.0322675109428288,1.12115139781563,0.615700786872883));
#12371=CARTESIAN_POINT('Origin',(0.3318563713692,1.12115139781563,0.6));
#12372=CARTESIAN_POINT('',(0.275700153393682,1.4152837823473,0.618237860411764));
#12373=CARTESIAN_POINT('Origin',(0.3318563713692,1.12115139781563,0.6));
#12374=CARTESIAN_POINT('Origin',(0.331856371369201,1.12115139781563,0.600000000000001));
#12375=CARTESIAN_POINT('Origin',(11.6681436286308,1.2964346619681,0.6));
#12376=CARTESIAN_POINT('',(11.6681436286308,1.2964346619681,0.9));
#12377=CARTESIAN_POINT('',(11.6974038588243,1.59451504727786,0.617085749108931));
#12378=CARTESIAN_POINT('Origin',(11.6681436286308,1.2964346619681,0.6));
#12379=CARTESIAN_POINT('',(11.9677324890572,1.2964346619681,0.615700786872884));
#12380=CARTESIAN_POINT('Origin',(11.6681436286308,1.2964346619681,0.6));
#12381=CARTESIAN_POINT('Origin',(11.6681436286308,1.2964346619681,0.6));
#12382=CARTESIAN_POINT('Origin',(0.3318563713692,-1.12115139781563,0.6));
#12383=CARTESIAN_POINT('',(0.3318563713692,-1.12115139781563,0.9));
#12384=CARTESIAN_POINT('',(0.27570015339368,-1.4152837823473,0.618237860411764));
#12385=CARTESIAN_POINT('Origin',(0.331856371369206,-1.12115139781563,0.6));
#12386=CARTESIAN_POINT('',(0.0322675109428289,-1.12115139781563,0.615700786872884));
#12387=CARTESIAN_POINT('Origin',(0.3318563713692,-1.12115139781563,0.6));
#12388=CARTESIAN_POINT('Origin',(0.331856371369201,-1.12115139781563,0.6));
#12389=CARTESIAN_POINT('Origin',(0.3318563713692,-0.7,0.6));
#12390=CARTESIAN_POINT('',(0.0322675109428288,-0.7,0.615700786872883));
#12391=CARTESIAN_POINT('',(0.3318563713692,-0.7,0.9));
#12392=CARTESIAN_POINT('Ctrl Pts',(0.243379792658812,-1.44768816351885,
-0.00386660544379547));
#12393=CARTESIAN_POINT('Ctrl Pts',(0.254153714020244,-1.43688644166428,
0.203501514337738));
#12394=CARTESIAN_POINT('Ctrl Pts',(0.264927169923045,-1.42608498030896,
0.410869669467268));
#12395=CARTESIAN_POINT('Ctrl Pts',(0.275700153393682,-1.4152837823473,0.618237860411764));
#12396=CARTESIAN_POINT('Ctrl Pts',(0.165985306518657,-1.43278556900406,
-0.000585522405354874));
#12397=CARTESIAN_POINT('Ctrl Pts',(0.176781886982148,-1.42196211044871,
0.206780297826791));
#12398=CARTESIAN_POINT('Ctrl Pts',(0.187577631459021,-1.41114055376332,
0.414146260476818));
#12399=CARTESIAN_POINT('Ctrl Pts',(0.198373523197449,-1.40031743725927,
0.621512129789107));
#12400=CARTESIAN_POINT('Ctrl Pts',(0.0420337764471552,-1.35067831466576,
0.00164062070145552));
#12401=CARTESIAN_POINT('Ctrl Pts',(0.0528811856485653,-1.33984924001505,
0.209003590924217));
#12402=CARTESIAN_POINT('Ctrl Pts',(0.0637288270387668,-1.3290196870647,
0.416366521726085));
#12403=CARTESIAN_POINT('Ctrl Pts',(0.0745760486629849,-1.31819094697801,
0.623729515932473));
#12404=CARTESIAN_POINT('Ctrl Pts',(-0.000174449685670057,-1.21258510413485,
-0.00332869829739982));
#12405=CARTESIAN_POINT('Ctrl Pts',(0.0106931634330696,-1.20178787588112,
0.204035045544629));
#12406=CARTESIAN_POINT('Ctrl Pts',(0.0215603573327632,-1.19099068058357,
0.411398812224037));
#12407=CARTESIAN_POINT('Ctrl Pts',(0.0324279732074593,-1.18019411246525,
0.618762589277523));
#12408=CARTESIAN_POINT('Ctrl Pts',(-0.000335035344191381,-1.15350137313465,
-0.00639285519773308));
#12409=CARTESIAN_POINT('Ctrl Pts',(0.0105324790023165,-1.1427176497384,
0.200971671503832));
#12410=CARTESIAN_POINT('Ctrl Pts',(0.0213999944262164,-1.13193432274319,
0.408336218763261));
#12411=CARTESIAN_POINT('Ctrl Pts',(0.0322675109428286,-1.12115139781563,
0.615700786872884));
#12412=CARTESIAN_POINT('Ctrl Pts',(0.243580684154575,-1.44748675362873,
-2.16840434497101E-17));
#12413=CARTESIAN_POINT('Ctrl Pts',(0.254287635915809,-1.43675217163244,
0.206079251738322));
#12414=CARTESIAN_POINT('Ctrl Pts',(0.264994127943615,-1.42601784692504,
0.412158538389471));
#12415=CARTESIAN_POINT('Ctrl Pts',(0.275700153393682,-1.4152837823473,0.618237860411764));
#12416=CARTESIAN_POINT('Ctrl Pts',(0.0322675109428286,-1.12115139781563,
0.615700786872884));
#12417=CARTESIAN_POINT('Ctrl Pts',(0.0215116728964671,-1.13182351356624,
0.410467170919192));
#12418=CARTESIAN_POINT('Ctrl Pts',(0.0107558359204751,-1.14249602316337,
0.205233575389367));
#12419=CARTESIAN_POINT('Ctrl Pts',(-1.41190227911925E-16,-1.15316892111333,
8.06646416329215E-17));
#12420=CARTESIAN_POINT('Origin',(11.6681436286308,-1.2964346619681,0.6));
#12421=CARTESIAN_POINT('',(11.9677324890572,-1.2964346619681,0.615700786872884));
#12422=CARTESIAN_POINT('',(11.6974038588243,-1.59451504727786,0.617085749108931));
#12423=CARTESIAN_POINT('Origin',(11.6681436286308,-1.2964346619681,0.600000000000001));
#12424=CARTESIAN_POINT('',(11.6681436286308,-1.2964346619681,0.9));
#12425=CARTESIAN_POINT('Origin',(11.6681436286308,-1.2964346619681,0.6));
#12426=CARTESIAN_POINT('Origin',(11.6681436286308,-1.2964346619681,0.6));
#12427=CARTESIAN_POINT('Origin',(11.6681436286308,0.8,0.6));
#12428=CARTESIAN_POINT('',(11.9677324890572,0.8,0.615700786872884));
#12429=CARTESIAN_POINT('',(11.6681436286308,0.8,0.9));
#12430=CARTESIAN_POINT('Ctrl Pts',(11.6681436286308,-1.2964346619681,0.9));
#12431=CARTESIAN_POINT('Ctrl Pts',(10.0505146497799,-1.45522470190849,0.9));
#12432=CARTESIAN_POINT('Ctrl Pts',(7.34698379851713,-1.66064017564263,0.9));
#12433=CARTESIAN_POINT('Ctrl Pts',(3.5507249968367,-1.5921338472202,0.9));
#12434=CARTESIAN_POINT('Ctrl Pts',(1.39628032950236,-1.32437289587156,0.9));
#12435=CARTESIAN_POINT('Ctrl Pts',(0.331856371369199,-1.12115139781563,
0.9));
#12436=CARTESIAN_POINT('Ctrl Pts',(11.6765943959699,-1.38252448313292,0.9));
#12437=CARTESIAN_POINT('Ctrl Pts',(10.0577014803155,-1.54155822929668,0.900004386952174));
#12438=CARTESIAN_POINT('Ctrl Pts',(7.35045927226653,-1.74750661992774,0.90000020513805));
#12439=CARTESIAN_POINT('Ctrl Pts',(3.54497585078588,-1.67885197560093,0.899998846478116));
#12440=CARTESIAN_POINT('Ctrl Pts',(1.38372480803625,-1.41002339692611,0.900007381454799));
#12441=CARTESIAN_POINT('Ctrl Pts',(0.315675209020016,-1.2059043252356,0.9));
#12442=CARTESIAN_POINT('Ctrl Pts',(11.6912432102654,-1.53175516862908,0.830242007927396));
#12443=CARTESIAN_POINT('Ctrl Pts',(10.070172518288,-1.69119563674726,0.830042231904815));
#12444=CARTESIAN_POINT('Ctrl Pts',(7.35645297288469,-1.89806162871739,0.829725685238203));
#12445=CARTESIAN_POINT('Ctrl Pts',(3.53503777381493,-1.8291593714544,0.829829026055289));
#12446=CARTESIAN_POINT('Ctrl Pts',(1.36192166831068,-1.55847530615989,0.830279056498203));
#12447=CARTESIAN_POINT('Ctrl Pts',(0.28762358730286,-1.35283178372728,0.830616544072481));
#12448=CARTESIAN_POINT('Ctrl Pts',(11.6970428895979,-1.59083777456472,0.681858145263203));
#12449=CARTESIAN_POINT('Ctrl Pts',(10.0750816081461,-1.75021732245097,0.681339641080976));
#12450=CARTESIAN_POINT('Ctrl Pts',(7.3588078744758,-1.95708146899443,0.680519979048775));
#12451=CARTESIAN_POINT('Ctrl Pts',(3.53113644431293,-1.88819699008302,0.68078748362792));
#12452=CARTESIAN_POINT('Ctrl Pts',(1.35331700817769,-1.61730376958615,0.681953432622034));
#12453=CARTESIAN_POINT('Ctrl Pts',(0.276437927844241,-1.41141950219787,
0.682830994206899));
#12454=CARTESIAN_POINT('Ctrl Pts',(11.6974038588243,-1.59451504727786,0.617085749108931));
#12455=CARTESIAN_POINT('Ctrl Pts',(10.0753786444688,-1.75377172884558,0.616473434532366));
#12456=CARTESIAN_POINT('Ctrl Pts',(7.35893161235257,-1.96044797105896,0.61550283428964));
#12457=CARTESIAN_POINT('Ctrl Pts',(3.53092277948893,-1.89162724517065,0.615818637525046));
#12458=CARTESIAN_POINT('Ctrl Pts',(1.35277799022997,-1.62098550016515,0.617200513836093));
#12459=CARTESIAN_POINT('Ctrl Pts',(0.27570015339368,-1.4152837823473,0.618237860411764));
#12460=CARTESIAN_POINT('Ctrl Pts',(0.27570015339368,-1.4152837823473,0.618237860411764));
#12461=CARTESIAN_POINT('Ctrl Pts',(1.35277799022997,-1.62098550016515,0.617200513836093));
#12462=CARTESIAN_POINT('Ctrl Pts',(3.53092277948893,-1.89162724517065,0.615818637525046));
#12463=CARTESIAN_POINT('Ctrl Pts',(7.35893161235257,-1.96044797105896,0.61550283428964));
#12464=CARTESIAN_POINT('Ctrl Pts',(10.0753786444688,-1.75377172884558,0.616473434532366));
#12465=CARTESIAN_POINT('Ctrl Pts',(11.6974038588243,-1.59451504727786,0.617085749108931));
#12466=CARTESIAN_POINT('Ctrl Pts',(11.6681436286308,-1.2964346619681,0.9));
#12467=CARTESIAN_POINT('Ctrl Pts',(10.0505146497799,-1.45522470190849,0.9));
#12468=CARTESIAN_POINT('Ctrl Pts',(7.34698379851713,-1.66064017564263,0.9));
#12469=CARTESIAN_POINT('Ctrl Pts',(3.5507249968367,-1.5921338472202,0.9));
#12470=CARTESIAN_POINT('Ctrl Pts',(1.39628032950236,-1.32437289587156,0.9));
#12471=CARTESIAN_POINT('Ctrl Pts',(0.331856371369199,-1.12115139781563,
0.9));
#12472=CARTESIAN_POINT('Ctrl Pts',(12.0003454972153,-1.32890342861544,-0.00659247958978532));
#12473=CARTESIAN_POINT('Ctrl Pts',(11.9894744951615,-1.31808026232082,0.200838596530835));
#12474=CARTESIAN_POINT('Ctrl Pts',(11.9786034924455,-1.30725733885828,0.408269685287046));
#12475=CARTESIAN_POINT('Ctrl Pts',(11.9677324890572,-1.2964346619681,0.615700786872884));
#12476=CARTESIAN_POINT('Ctrl Pts',(12.000116620981,-1.41283311850955,-0.00222526087931226));
#12477=CARTESIAN_POINT('Ctrl Pts',(11.9892453109784,-1.40200002127642,0.205205215027088));
#12478=CARTESIAN_POINT('Ctrl Pts',(11.9783750177566,-1.39116761830557,0.412635780645844));
#12479=CARTESIAN_POINT('Ctrl Pts',(11.9675037034976,-1.38033490526933,0.620066275407343));
#12480=CARTESIAN_POINT('Ctrl Pts',(11.9341774721098,-1.5584705948029,0.00191796595980313));
#12481=CARTESIAN_POINT('Ctrl Pts',(11.9233226835938,-1.54762133657986,0.209348350794306));
#12482=CARTESIAN_POINT('Ctrl Pts',(11.9124678718222,-1.53677206634062,0.416778732304926));
#12483=CARTESIAN_POINT('Ctrl Pts',(11.9016132473252,-1.52592301942363,0.624209134118803));
#12484=CARTESIAN_POINT('Ctrl Pts',(11.7925116537096,-1.62071287545028,-0.0022587989925734));
#12485=CARTESIAN_POINT('Ctrl Pts',(11.7816834491585,-1.6098745265243,0.205173499361722));
#12486=CARTESIAN_POINT('Ctrl Pts',(11.7708551999607,-1.59903658749835,0.41260581547062));
#12487=CARTESIAN_POINT('Ctrl Pts',(11.760027440985,-1.58819854843564,0.620038149897102));
#12488=CARTESIAN_POINT('Ctrl Pts',(11.7298629188572,-1.62699926142283,-0.0052140742384003));
#12489=CARTESIAN_POINT('Ctrl Pts',(11.7190429637906,-1.61617098622686,0.202219177289036));
#12490=CARTESIAN_POINT('Ctrl Pts',(11.708223275703,-1.60534291388117,0.409652451626141));
#12491=CARTESIAN_POINT('Ctrl Pts',(11.6974038588243,-1.59451504727786,0.617085749108931));
#12492=CARTESIAN_POINT('Ctrl Pts',(12.,-1.32855945177638,-1.94722710178397E-16));
#12493=CARTESIAN_POINT('Ctrl Pts',(11.9892441636707,-1.31785094954632,0.205233583190348));
#12494=CARTESIAN_POINT('Ctrl Pts',(11.978488326693,-1.30714268506935,0.410467178751997));
#12495=CARTESIAN_POINT('Ctrl Pts',(11.9677324890572,-1.2964346619681,0.615700786872884));
#12496=CARTESIAN_POINT('Ctrl Pts',(11.6974038588243,-1.59451504727786,0.617085749108931));
#12497=CARTESIAN_POINT('Ctrl Pts',(11.7081326228587,-1.605252190239,0.41139047675572));
#12498=CARTESIAN_POINT('Ctrl Pts',(11.7188616535763,-1.61598953550924,0.205695227161956));
#12499=CARTESIAN_POINT('Ctrl Pts',(11.7295909468525,-1.62672708026858,8.73866951023317E-17));
#12500=CARTESIAN_POINT('Ctrl Pts',(11.7298546566854,1.62699099289774,-0.00505567716946009));
#12501=CARTESIAN_POINT('Ctrl Pts',(11.719037455812,1.61616547398006,0.202324775346606));
#12502=CARTESIAN_POINT('Ctrl Pts',(11.7082205217827,1.60534015781013,0.409705250660816));
#12503=CARTESIAN_POINT('Ctrl Pts',(11.6974038588243,1.59451504727786,0.617085749108931));
#12504=CARTESIAN_POINT('Ctrl Pts',(11.8133862946664,1.61860913476435,-0.00111531114554236));
#12505=CARTESIAN_POINT('Ctrl Pts',(11.8025579038448,1.6077699189899,0.206263846261978));
#12506=CARTESIAN_POINT('Ctrl Pts',(11.7917299466398,1.59693199028804,0.41364309356145));
#12507=CARTESIAN_POINT('Ctrl Pts',(11.7809019683719,1.58609304882157,0.621022283493159));
#12508=CARTESIAN_POINT('Ctrl Pts',(11.9519653779615,1.53884931758497,0.00198566945999789));
#12509=CARTESIAN_POINT('Ctrl Pts',(11.9411087765487,1.52800449744246,0.209363119024413));
#12510=CARTESIAN_POINT('Ctrl Pts',(11.9302521502216,1.51715965702667,0.416740564833343));
#12511=CARTESIAN_POINT('Ctrl Pts',(11.9193956662674,1.50631506689811,0.624118030142866));
#12512=CARTESIAN_POINT('Ctrl Pts',(12.0001655389052,1.39184242582033,-0.00315867047762133));
#12513=CARTESIAN_POINT('Ctrl Pts',(11.9892972278067,1.38101476165208,0.204219175612729));
#12514=CARTESIAN_POINT('Ctrl Pts',(11.9784292129672,1.37018709651964,0.41159703650799));
#12515=CARTESIAN_POINT('Ctrl Pts',(11.9675608998875,1.35935984444403,0.618974903273729));
#12516=CARTESIAN_POINT('Ctrl Pts',(12.0003371960637,1.32889516399154,-0.00643408418199817));
#12517=CARTESIAN_POINT('Ctrl Pts',(11.9894689610601,1.31807475269516,0.200944193475792));
#12518=CARTESIAN_POINT('Ctrl Pts',(11.9786007253947,1.3072545841082,0.408322483762789));
#12519=CARTESIAN_POINT('Ctrl Pts',(11.9677324890572,1.2964346619681,0.615700786872884));
#12520=CARTESIAN_POINT('Ctrl Pts',(11.7295909468525,1.62672708026857,-8.50014503228635E-17));
#12521=CARTESIAN_POINT('Ctrl Pts',(11.7188616535763,1.61598953550924,0.205695227161956));
#12522=CARTESIAN_POINT('Ctrl Pts',(11.7081326228587,1.605252190239,0.411390476755719));
#12523=CARTESIAN_POINT('Ctrl Pts',(11.6974038588243,1.59451504727786,0.617085749108931));
#12524=CARTESIAN_POINT('Ctrl Pts',(11.9677324890572,1.2964346619681,0.615700786872884));
#12525=CARTESIAN_POINT('Ctrl Pts',(11.978488326693,1.30714268506935,0.410467178751997));
#12526=CARTESIAN_POINT('Ctrl Pts',(11.9892441636707,1.31785094954633,0.205233583190349));
#12527=CARTESIAN_POINT('Ctrl Pts',(12.,1.32855945177638,-2.38524477946811E-17));
#12528=CARTESIAN_POINT('Ctrl Pts',(0.3318563713692,1.12115139781563,0.9));
#12529=CARTESIAN_POINT('Ctrl Pts',(1.92849230856897,1.42598364489954,0.9));
#12530=CARTESIAN_POINT('Ctrl Pts',(5.71993880054687,1.76935652211139,0.9));
#12531=CARTESIAN_POINT('Ctrl Pts',(9.51130499016288,1.50815471522196,0.9));
#12532=CARTESIAN_POINT('Ctrl Pts',(11.6681436286308,1.2964346619681,0.9));
#12533=CARTESIAN_POINT('Ctrl Pts',(0.315675209020018,1.2059043252356,0.9));
#12534=CARTESIAN_POINT('Ctrl Pts',(1.91774960754439,1.51208293277137,0.900011072182198));
#12535=CARTESIAN_POINT('Ctrl Pts',(5.72069615836457,1.85663493780214,0.899990666655967));
#12536=CARTESIAN_POINT('Ctrl Pts',(9.5180705084307,1.59456947801794,0.900005849269565));
#12537=CARTESIAN_POINT('Ctrl Pts',(11.6765943959699,1.38252448313292,0.9));
#12538=CARTESIAN_POINT('Ctrl Pts',(0.287623587302861,1.35283178372728,0.83061654407248));
#12539=CARTESIAN_POINT('Ctrl Pts',(1.89907070881462,1.6612970673762,0.830110312711064));
#12540=CARTESIAN_POINT('Ctrl Pts',(5.72203120258494,2.00791989451774,0.829536565111056));
#12541=CARTESIAN_POINT('Ctrl Pts',(9.52981562096212,1.74434245945332,0.829975639897288));
#12542=CARTESIAN_POINT('Ctrl Pts',(11.6912432102654,1.53175516862908,0.830242007927395));
#12543=CARTESIAN_POINT('Ctrl Pts',(0.276437927844243,1.41141950219787,0.682830994206899));
#12544=CARTESIAN_POINT('Ctrl Pts',(1.89175654834445,1.7202459032803,0.681514651829601));
#12545=CARTESIAN_POINT('Ctrl Pts',(5.72254254462207,2.06699613896002,0.680031275065471));
#12546=CARTESIAN_POINT('Ctrl Pts',(9.53442784766217,1.80334383841306,0.681166806353567));
#12547=CARTESIAN_POINT('Ctrl Pts',(11.6970428895979,1.59083777456472,0.681858145263204));
#12548=CARTESIAN_POINT('Ctrl Pts',(0.275700153393682,1.4152837823473,0.618237860411764));
#12549=CARTESIAN_POINT('Ctrl Pts',(1.89131690864814,1.72383635907408,0.616681840548257));
#12550=CARTESIAN_POINT('Ctrl Pts',(5.72257555688819,2.07025489722917,0.614922376024419));
#12551=CARTESIAN_POINT('Ctrl Pts',(9.53470357301702,1.80685728936816,0.616269329673511));
#12552=CARTESIAN_POINT('Ctrl Pts',(11.6974038588243,1.59451504727786,0.617085749108931));
#12553=CARTESIAN_POINT('Ctrl Pts',(11.6974038588243,1.59451504727786,0.617085749108931));
#12554=CARTESIAN_POINT('Ctrl Pts',(9.53470357301702,1.80685728936816,0.616269329673511));
#12555=CARTESIAN_POINT('Ctrl Pts',(5.72257555688819,2.07025489722917,0.614922376024419));
#12556=CARTESIAN_POINT('Ctrl Pts',(1.89131690864814,1.72383635907408,0.616681840548257));
#12557=CARTESIAN_POINT('Ctrl Pts',(0.275700153393682,1.4152837823473,0.618237860411764));
#12558=CARTESIAN_POINT('Ctrl Pts',(0.3318563713692,1.12115139781563,0.9));
#12559=CARTESIAN_POINT('Ctrl Pts',(1.92849230856897,1.42598364489954,0.9));
#12560=CARTESIAN_POINT('Ctrl Pts',(5.71993880054687,1.76935652211139,0.9));
#12561=CARTESIAN_POINT('Ctrl Pts',(9.51130499016288,1.50815471522196,0.9));
#12562=CARTESIAN_POINT('Ctrl Pts',(11.6681436286308,1.2964346619681,0.9));
#12563=CARTESIAN_POINT('Ctrl Pts',(-0.000343174493958709,1.15350944952984,
-0.00654815942696785));
#12564=CARTESIAN_POINT('Ctrl Pts',(0.0105270529019337,1.14272303380391,
0.200868135340743));
#12565=CARTESIAN_POINT('Ctrl Pts',(0.0213972813757523,1.13193701467556,
0.408284450676511));
#12566=CARTESIAN_POINT('Ctrl Pts',(0.0322675109428289,1.12115139781563,
0.615700786872884));
#12567=CARTESIAN_POINT('Ctrl Pts',(-0.000129060241737355,1.23228777111366,
-0.0024626161135415));
#12568=CARTESIAN_POINT('Ctrl Pts',(0.0107416412387167,1.22148297235423,
0.204952596860618));
#12569=CARTESIAN_POINT('Ctrl Pts',(0.0216107531875107,1.21067920461451,
0.412367946918899));
#12570=CARTESIAN_POINT('Ctrl Pts',(0.0324814606290031,1.19987501734845,
0.61978319007907));
#12571=CARTESIAN_POINT('Ctrl Pts',(0.0574602827844584,1.36931747586956,
0.00164530659801973));
#12572=CARTESIAN_POINT('Ctrl Pts',(0.0683025556324749,1.35848226928888,
0.209060253413207));
#12573=CARTESIAN_POINT('Ctrl Pts',(0.079145272670006,1.34764679267913,0.416475160658282));
#12574=CARTESIAN_POINT('Ctrl Pts',(0.0899872847341513,1.33681188280878,
0.62389013300849));
#12575=CARTESIAN_POINT('Ctrl Pts',(0.185325846363896,1.43651931939441,-0.00156109881554352));
#12576=CARTESIAN_POINT('Ctrl Pts',(0.196119220517603,1.4256988926218,0.205857093047737));
#12577=CARTESIAN_POINT('Ctrl Pts',(0.20691256009293,1.41487906031557,0.413275315721495));
#12578=CARTESIAN_POINT('Ctrl Pts',(0.217705180746507,1.40405902353128,0.620693562444772));
#12579=CARTESIAN_POINT('Ctrl Pts',(0.243371723604776,1.44769625339383,-0.00402191236404));
#12580=CARTESIAN_POINT('Ctrl Pts',(0.254148334883323,1.43689183478419,0.203397976373256));
#12581=CARTESIAN_POINT('Ctrl Pts',(0.264924480472538,1.42608767680315,0.410817900476086));
#12582=CARTESIAN_POINT('Ctrl Pts',(0.275700153393682,1.4152837823473,0.618237860411764));
#12583=CARTESIAN_POINT('Ctrl Pts',(-1.23734572934908E-17,1.15316892111333,
-8.67361737988404E-19));
#12584=CARTESIAN_POINT('Ctrl Pts',(0.0107558359204753,1.14249602316336,
0.205233575389367));
#12585=CARTESIAN_POINT('Ctrl Pts',(0.0215116728964674,1.13182351356624,
0.410467170919192));
#12586=CARTESIAN_POINT('Ctrl Pts',(0.0322675109428289,1.12115139781563,
0.615700786872884));
#12587=CARTESIAN_POINT('Ctrl Pts',(0.275700153393682,1.4152837823473,0.618237860411764));
#12588=CARTESIAN_POINT('Ctrl Pts',(0.264994127943615,1.42601784692504,0.412158538389472));
#12589=CARTESIAN_POINT('Ctrl Pts',(0.254287635915814,1.43675217163244,0.206079251738322));
#12590=CARTESIAN_POINT('Ctrl Pts',(0.243580684154575,1.44748675362873,-1.9298798670242E-17));
#12591=CARTESIAN_POINT('Ctrl Pts',(11.7295909468525,-1.62672708026858,0.));
#12592=CARTESIAN_POINT('Ctrl Pts',(11.7192775324813,-1.61592692249094,0.206079286804135));
#12593=CARTESIAN_POINT('Ctrl Pts',(11.70896411811,-1.6051267647133,0.41215857360827));
#12594=CARTESIAN_POINT('Ctrl Pts',(11.6986507037388,-1.59432660693566,0.618237860412405));
#12595=CARTESIAN_POINT('Ctrl Pts',(7.90092085928651,-2.00057770191527,0.));
#12596=CARTESIAN_POINT('Ctrl Pts',(7.89749915175266,-1.98977754413763,0.206079286804135));
#12597=CARTESIAN_POINT('Ctrl Pts',(7.89407744421881,-1.97897738636,0.41215857360827));
#12598=CARTESIAN_POINT('Ctrl Pts',(7.89065573668496,-1.96817722858236,0.618237860412405));
#12599=CARTESIAN_POINT('Ctrl Pts',(4.07225077172054,-2.17467835246083,0.));
#12600=CARTESIAN_POINT('Ctrl Pts',(4.07572077102407,-2.16387819468319,0.206079286804135));
#12601=CARTESIAN_POINT('Ctrl Pts',(4.07919077032759,-2.15307803690555,0.41215857360827));
#12602=CARTESIAN_POINT('Ctrl Pts',(4.08266076963111,-2.14227787912792,0.618237860412405));
#12603=CARTESIAN_POINT('Ctrl Pts',(0.243580684154574,-1.44748675362873,
0.));
#12604=CARTESIAN_POINT('Ctrl Pts',(0.253942390295469,-1.43668659585109,
0.206079286804135));
#12605=CARTESIAN_POINT('Ctrl Pts',(0.264304096436365,-1.42588643807345,
0.41215857360827));
#12606=CARTESIAN_POINT('Ctrl Pts',(0.27466580257726,-1.41508628029581,0.618237860412405));
#12607=CARTESIAN_POINT('Origin',(0.,-1.4,0.));
#12608=CARTESIAN_POINT('Origin',(6.08012166120517,1.06803409199199E-16,
0.9));
#12609=CARTESIAN_POINT('Ctrl Pts',(0.243580684154574,1.44748675362873,0.));
#12610=CARTESIAN_POINT('Ctrl Pts',(0.253942390295469,1.43668659585109,0.206079286804135));
#12611=CARTESIAN_POINT('Ctrl Pts',(0.264304096436365,1.42588643807345,0.41215857360827));
#12612=CARTESIAN_POINT('Ctrl Pts',(0.27466580257726,1.41508628029581,0.618237860412405));
#12613=CARTESIAN_POINT('Ctrl Pts',(4.07225077172054,2.17467835246083,0.));
#12614=CARTESIAN_POINT('Ctrl Pts',(4.07572077102407,2.16387819468319,0.206079286804135));
#12615=CARTESIAN_POINT('Ctrl Pts',(4.07919077032759,2.15307803690555,0.41215857360827));
#12616=CARTESIAN_POINT('Ctrl Pts',(4.08266076963111,2.14227787912792,0.618237860412405));
#12617=CARTESIAN_POINT('Ctrl Pts',(7.90092085928651,2.00057770191527,0.));
#12618=CARTESIAN_POINT('Ctrl Pts',(7.89749915175266,1.98977754413763,0.206079286804135));
#12619=CARTESIAN_POINT('Ctrl Pts',(7.89407744421881,1.97897738636,0.41215857360827));
#12620=CARTESIAN_POINT('Ctrl Pts',(7.89065573668496,1.96817722858236,0.618237860412405));
#12621=CARTESIAN_POINT('Ctrl Pts',(11.7295909468525,1.62672708026858,0.));
#12622=CARTESIAN_POINT('Ctrl Pts',(11.7192775324813,1.61592692249094,0.206079286804135));
#12623=CARTESIAN_POINT('Ctrl Pts',(11.70896411811,1.6051267647133,0.41215857360827));
#12624=CARTESIAN_POINT('Ctrl Pts',(11.6986507037388,1.59432660693566,0.618237860412405));
#12625=CARTESIAN_POINT('Origin',(12.,1.6,0.));
#12626=CARTESIAN_POINT('',(0.,0.,0.));
#12627=CARTESIAN_POINT('Origin',(2.,0.,1.));
#12628=CARTESIAN_POINT('',(1.65,4.28626379701574E-17,1.1));
#12629=CARTESIAN_POINT('Origin',(2.,0.,1.1));
#12630=CARTESIAN_POINT('',(1.65,4.28626379701574E-17,0.9));
#12631=CARTESIAN_POINT('',(1.65,4.28626379701574E-17,1.));
#12632=CARTESIAN_POINT('Origin',(2.,0.,0.9));
#12633=CARTESIAN_POINT('Origin',(10.,0.,1.));
#12634=CARTESIAN_POINT('',(9.65,4.28626379701574E-17,1.1));
#12635=CARTESIAN_POINT('Origin',(10.,0.,1.1));
#12636=CARTESIAN_POINT('',(9.65,4.28626379701574E-17,0.9));
#12637=CARTESIAN_POINT('',(9.65,4.28626379701574E-17,1.));
#12638=CARTESIAN_POINT('Origin',(10.,0.,0.9));
#12639=CARTESIAN_POINT('Origin',(9.,1.,0.7));
#12640=CARTESIAN_POINT('',(8.75,1.,0.7));
#12641=CARTESIAN_POINT('Origin',(9.,1.,0.7));
#12642=CARTESIAN_POINT('',(8.85,1.,0.7));
#12643=CARTESIAN_POINT('Origin',(9.,1.,0.7));
#12644=CARTESIAN_POINT('Origin',(9.,1.,0.7));
#12645=CARTESIAN_POINT('',(8.75,1.,0.6));
#12646=CARTESIAN_POINT('Origin',(9.,1.,0.6));
#12647=CARTESIAN_POINT('',(8.75,1.,0.7));
#12648=CARTESIAN_POINT('Origin',(9.,1.,0.6));
#12649=CARTESIAN_POINT('Origin',(3.,-1.,0.7));
#12650=CARTESIAN_POINT('',(2.75,-1.,0.7));
#12651=CARTESIAN_POINT('Origin',(3.,-1.,0.7));
#12652=CARTESIAN_POINT('',(2.85,-1.,0.7));
#12653=CARTESIAN_POINT('Origin',(3.,-1.,0.7));
#12654=CARTESIAN_POINT('Origin',(3.,-1.,0.7));
#12655=CARTESIAN_POINT('',(2.75,-1.,0.6));
#12656=CARTESIAN_POINT('Origin',(3.,-1.,0.6));
#12657=CARTESIAN_POINT('',(2.75,-1.,0.7));
#12658=CARTESIAN_POINT('Origin',(3.,-1.,0.6));
#12659=CARTESIAN_POINT('Origin',(3.,1.,0.7));
#12660=CARTESIAN_POINT('',(2.75,1.,0.7));
#12661=CARTESIAN_POINT('Origin',(3.,1.,0.7));
#12662=CARTESIAN_POINT('',(2.85,1.,0.7));
#12663=CARTESIAN_POINT('Origin',(3.,1.,0.7));
#12664=CARTESIAN_POINT('Origin',(3.,1.,0.7));
#12665=CARTESIAN_POINT('',(2.75,1.,0.6));
#12666=CARTESIAN_POINT('Origin',(3.,1.,0.6));
#12667=CARTESIAN_POINT('',(2.75,1.,0.7));
#12668=CARTESIAN_POINT('Origin',(3.,1.,0.6));
#12669=CARTESIAN_POINT('Origin',(9.,-1.,0.7));
#12670=CARTESIAN_POINT('',(8.75,-1.,0.7));
#12671=CARTESIAN_POINT('Origin',(9.,-1.,0.7));
#12672=CARTESIAN_POINT('',(8.85,-1.,0.7));
#12673=CARTESIAN_POINT('Origin',(9.,-1.,0.7));
#12674=CARTESIAN_POINT('Origin',(9.,-1.,0.7));
#12675=CARTESIAN_POINT('',(8.75,-1.,0.6));
#12676=CARTESIAN_POINT('Origin',(9.,-1.,0.6));
#12677=CARTESIAN_POINT('',(8.75,-1.,0.7));
#12678=CARTESIAN_POINT('Origin',(9.,-1.,0.6));
#12679=CARTESIAN_POINT('Origin',(9.,1.,0.9));
#12680=CARTESIAN_POINT('',(8.85,1.,0.9));
#12681=CARTESIAN_POINT('',(8.85,1.,0.9));
#12682=CARTESIAN_POINT('Origin',(9.,1.,0.9));
#12683=CARTESIAN_POINT('Origin',(3.,-1.,0.9));
#12684=CARTESIAN_POINT('',(2.85,-1.,0.9));
#12685=CARTESIAN_POINT('',(2.85,-1.,0.9));
#12686=CARTESIAN_POINT('Origin',(3.,-1.,0.9));
#12687=CARTESIAN_POINT('Origin',(3.,1.,0.9));
#12688=CARTESIAN_POINT('',(2.85,1.,0.9));
#12689=CARTESIAN_POINT('',(2.85,1.,0.9));
#12690=CARTESIAN_POINT('Origin',(3.,1.,0.9));
#12691=CARTESIAN_POINT('Origin',(9.,-1.,0.9));
#12692=CARTESIAN_POINT('',(8.85,-1.,0.9));
#12693=CARTESIAN_POINT('',(8.85,-1.,0.9));
#12694=CARTESIAN_POINT('Origin',(9.,-1.,0.9));
#12695=CARTESIAN_POINT('Ctrl Pts',(11.5038445323837,1.18103800495499,1.1));
#12696=CARTESIAN_POINT('Ctrl Pts',(11.5184054935931,1.17950950960121,1.1));
#12697=CARTESIAN_POINT('Ctrl Pts',(11.5512741038969,1.16492409601325,1.1));
#12698=CARTESIAN_POINT('Ctrl Pts',(11.5664342774515,1.13103804392606,1.1));
#12699=CARTESIAN_POINT('Ctrl Pts',(11.5664342774515,1.11151675574496,1.1));
#12700=CARTESIAN_POINT('Ctrl Pts',(11.5062520964801,1.2039732708886,1.1));
#12701=CARTESIAN_POINT('Ctrl Pts',(11.5256097704488,1.20178950015253,1.09999449529541));
#12702=CARTESIAN_POINT('Ctrl Pts',(11.5690795528293,1.18226331832779,1.09998611288251));
#12703=CARTESIAN_POINT('Ctrl Pts',(11.5893469235372,1.13750635859412,1.09999170314796));
#12704=CARTESIAN_POINT('Ctrl Pts',(11.5895723566779,1.11151675574496,1.1));
#12705=CARTESIAN_POINT('Ctrl Pts',(11.5104252001437,1.2437276609947,1.08142124563721));
#12706=CARTESIAN_POINT('Ctrl Pts',(11.5380451995806,1.2404317701584,1.0816749051734));
#12707=CARTESIAN_POINT('Ctrl Pts',(11.5998825216457,1.21232138637678,1.08202590066027));
#12708=CARTESIAN_POINT('Ctrl Pts',(11.629084458256,1.14864330516641,1.08167049691811));
#12709=CARTESIAN_POINT('Ctrl Pts',(11.629673151989,1.11151675574496,1.08129017730416));
#12710=CARTESIAN_POINT('Ctrl Pts',(11.5120790720623,1.25948300155991,1.0418569252725));
#12711=CARTESIAN_POINT('Ctrl Pts',(11.5430287132786,1.25602537746711,1.04251419789099));
#12712=CARTESIAN_POINT('Ctrl Pts',(11.6126593164611,1.22478248685392,1.04343302714342));
#12713=CARTESIAN_POINT('Ctrl Pts',(11.6451104499416,1.15305025146974,1.04249969645955));
#12714=CARTESIAN_POINT('Ctrl Pts',(11.6454164251054,1.11151675574496,1.0415166534692));
#12715=CARTESIAN_POINT('Ctrl Pts',(11.5121826600865,1.26046981594516,1.0245894475956));
#12716=CARTESIAN_POINT('Ctrl Pts',(11.5433440226796,1.25715387309455,1.02536599531596));
#12717=CARTESIAN_POINT('Ctrl Pts',(11.6137195683385,1.22584236729999,1.02645725900057));
#12718=CARTESIAN_POINT('Ctrl Pts',(11.6462638499073,1.15328744881755,1.02534682499181));
#12719=CARTESIAN_POINT('Ctrl Pts',(11.6463246402318,1.11151675574496,1.02418687649944));
#12720=CARTESIAN_POINT('',(11.5664342774515,1.11151675574496,1.1));
#12721=CARTESIAN_POINT('',(11.6463246402318,1.11151675574496,1.02418687649943));
#12722=CARTESIAN_POINT('Origin',(11.5664342774515,1.11151675574496,1.02));
#12723=CARTESIAN_POINT('',(11.5121826600865,1.26046981594516,1.0245894475956));
#12724=CARTESIAN_POINT('Ctrl Pts',(11.6463246402318,1.11151675574496,1.02418687649944));
#12725=CARTESIAN_POINT('Ctrl Pts',(11.6462638499073,1.15328744881755,1.02534682499181));
#12726=CARTESIAN_POINT('Ctrl Pts',(11.6137195683385,1.22584236729999,1.02645725900057));
#12727=CARTESIAN_POINT('Ctrl Pts',(11.5433440226796,1.25715387309455,1.02536599531596));
#12728=CARTESIAN_POINT('Ctrl Pts',(11.5121826600865,1.26046981594516,1.0245894475956));
#12729=CARTESIAN_POINT('',(11.5038445323837,1.18103800495499,1.1));
#12730=CARTESIAN_POINT('Origin',(11.5038445323837,1.18103800495499,1.02));
#12731=CARTESIAN_POINT('Ctrl Pts',(11.5038445323837,1.18103800495499,1.1));
#12732=CARTESIAN_POINT('Ctrl Pts',(11.5184054935931,1.17950950960121,1.1));
#12733=CARTESIAN_POINT('Ctrl Pts',(11.5512741038969,1.16492409601325,1.1));
#12734=CARTESIAN_POINT('Ctrl Pts',(11.5664342774515,1.13103804392606,1.1));
#12735=CARTESIAN_POINT('Ctrl Pts',(11.5664342774515,1.11151675574496,1.1));
#12736=CARTESIAN_POINT('Origin',(11.5664342774515,0.626416499322631,1.02));
#12737=CARTESIAN_POINT('',(11.5664342774515,-1.11151675574496,1.1));
#12738=CARTESIAN_POINT('',(11.6463246402318,-1.11151675574496,1.02418687649944));
#12739=CARTESIAN_POINT('Origin',(11.5664342774515,-1.11151675574496,1.02));
#12740=CARTESIAN_POINT('',(11.6463246402318,0.626416499322631,1.02418687649944));
#12741=CARTESIAN_POINT('',(11.5664342774515,0.626416499322631,1.1));
#12742=CARTESIAN_POINT('Ctrl Pts',(11.5664342774515,-1.11151675574496,1.1));
#12743=CARTESIAN_POINT('Ctrl Pts',(11.5664342774515,-1.12615772189446,1.1));
#12744=CARTESIAN_POINT('Ctrl Pts',(11.5553715698491,-1.16037133170262,1.1));
#12745=CARTESIAN_POINT('Ctrl Pts',(11.5232591473477,-1.17900001114805,1.1));
#12746=CARTESIAN_POINT('Ctrl Pts',(11.5038445323837,-1.181038004955,1.1));
#12747=CARTESIAN_POINT('Ctrl Pts',(11.5895723566779,-1.11151675574496,1.1));
#12748=CARTESIAN_POINT('Ctrl Pts',(11.5894032818222,-1.13100895790003,1.09999377736097));
#12749=CARTESIAN_POINT('Ctrl Pts',(11.5744722352599,-1.17628172883974,1.09998542409303));
#12750=CARTESIAN_POINT('Ctrl Pts',(11.5320623284624,-1.20106157657112,1.09999266039387));
#12751=CARTESIAN_POINT('Ctrl Pts',(11.5062520964801,-1.2039732708886,1.1));
#12752=CARTESIAN_POINT('Ctrl Pts',(11.6296731519891,-1.11151675574496,1.0812901773042));
#12753=CARTESIAN_POINT('Ctrl Pts',(11.6292316316889,-1.13936166783705,1.08157541701493));
#12754=CARTESIAN_POINT('Ctrl Pts',(11.6075809177182,-1.20379599023677,1.08201780166247));
#12755=CARTESIAN_POINT('Ctrl Pts',(11.547251866094,-1.23933313987557,1.08175945835248));
#12756=CARTESIAN_POINT('Ctrl Pts',(11.5104252001437,-1.24372766099475,1.08142124563725));
#12757=CARTESIAN_POINT('Ctrl Pts',(11.6454164251054,-1.11151675574496,1.0415166534692));
#12758=CARTESIAN_POINT('Ctrl Pts',(11.6451869437323,-1.14266687756763,1.04225393571265));
#12759=CARTESIAN_POINT('Ctrl Pts',(11.6213248916312,-1.21516855113593,1.04341114660737));
#12760=CARTESIAN_POINT('Ctrl Pts',(11.5533452603892,-1.25487283609854,1.04273328876464));
#12761=CARTESIAN_POINT('Ctrl Pts',(11.5120790720623,-1.25948300155991,1.0418569252725));
#12762=CARTESIAN_POINT('Ctrl Pts',(11.6463246402318,-1.11151675574496,1.02418687649944));
#12763=CARTESIAN_POINT('Ctrl Pts',(11.6462790474884,-1.14284477557865,1.02505683786953));
#12764=CARTESIAN_POINT('Ctrl Pts',(11.6225012384517,-1.21608782625165,1.02643081388051));
#12765=CARTESIAN_POINT('Ctrl Pts',(11.5537311435827,-1.25604855880689,1.02562484455705));
#12766=CARTESIAN_POINT('Ctrl Pts',(11.5121826600865,-1.26046981594517,1.0245894475956));
#12767=CARTESIAN_POINT('',(11.5038445323837,-1.181038004955,1.1));
#12768=CARTESIAN_POINT('',(11.5121826600865,-1.26046981594517,1.02458944759559));
#12769=CARTESIAN_POINT('Origin',(11.5038445323837,-1.181038004955,1.02));
#12770=CARTESIAN_POINT('Ctrl Pts',(11.5121826600865,-1.26046981594517,1.0245894475956));
#12771=CARTESIAN_POINT('Ctrl Pts',(11.5537311435827,-1.25604855880689,1.02562484455705));
#12772=CARTESIAN_POINT('Ctrl Pts',(11.6225012384517,-1.21608782625165,1.02643081388051));
#12773=CARTESIAN_POINT('Ctrl Pts',(11.6462790474884,-1.14284477557865,1.02505683786953));
#12774=CARTESIAN_POINT('Ctrl Pts',(11.6463246402318,-1.11151675574496,1.02418687649944));
#12775=CARTESIAN_POINT('Ctrl Pts',(11.5664342774515,-1.11151675574496,1.1));
#12776=CARTESIAN_POINT('Ctrl Pts',(11.5664342774515,-1.12615772189446,1.1));
#12777=CARTESIAN_POINT('Ctrl Pts',(11.5553715698491,-1.16037133170262,1.1));
#12778=CARTESIAN_POINT('Ctrl Pts',(11.5232591473477,-1.17900001114805,1.1));
#12779=CARTESIAN_POINT('Ctrl Pts',(11.5038445323837,-1.181038004955,1.1));
#12780=CARTESIAN_POINT('Ctrl Pts',(11.5038445323836,-1.181038004955,1.1));
#12781=CARTESIAN_POINT('Ctrl Pts',(9.93221394244152,-1.34601544154236,1.1));
#12782=CARTESIAN_POINT('Ctrl Pts',(7.3047417451522,-1.56119993769491,1.1));
#12783=CARTESIAN_POINT('Ctrl Pts',(3.61332606662357,-1.48882378722464,1.1));
#12784=CARTESIAN_POINT('Ctrl Pts',(1.52093096174237,-1.20661833758759,1.1));
#12785=CARTESIAN_POINT('Ctrl Pts',(0.489277774073836,-0.993132359214002,
1.1));
#12786=CARTESIAN_POINT('Ctrl Pts',(11.5062520964801,-1.2039732708886,1.1));
#12787=CARTESIAN_POINT('Ctrl Pts',(9.93427206726409,-1.36902193231914,1.10000125302342));
#12788=CARTESIAN_POINT('Ctrl Pts',(7.30574352860662,-1.58436797372637,1.10000007151586));
#12789=CARTESIAN_POINT('Ctrl Pts',(3.61166276511536,-1.51194672535434,1.09999968963322));
#12790=CARTESIAN_POINT('Ctrl Pts',(1.51730587435546,-1.22941181706429,1.10000211650891));
#12791=CARTESIAN_POINT('Ctrl Pts',(0.48461766586479,-1.01565194352286,1.1));
#12792=CARTESIAN_POINT('Ctrl Pts',(11.5104252017938,-1.24372767671385,1.08142125970198));
#12793=CARTESIAN_POINT('Ctrl Pts',(9.93784299858723,-1.40889527428921,1.08136351975694));
#12794=CARTESIAN_POINT('Ctrl Pts',(7.3074712357333,-1.62451940065184,1.08127113650551));
#12795=CARTESIAN_POINT('Ctrl Pts',(3.60878747433083,-1.55202277432172,1.08130174433006));
#12796=CARTESIAN_POINT('Ctrl Pts',(1.51101154909588,-1.26891547398152,1.08143311272106));
#12797=CARTESIAN_POINT('Ctrl Pts',(0.476539293980871,-1.05469000198791,
1.08153107638517));
#12798=CARTESIAN_POINT('Ctrl Pts',(11.5120790720622,-1.25948300155992,1.0418569252725));
#12799=CARTESIAN_POINT('Ctrl Pts',(9.93924961011084,-1.42463380902671,1.04170731179674));
#12800=CARTESIAN_POINT('Ctrl Pts',(7.30815001459807,-1.64026117966461,1.0414672686166));
#12801=CARTESIAN_POINT('Ctrl Pts',(3.60765874156876,-1.56776897899067,1.04154646081959));
#12802=CARTESIAN_POINT('Ctrl Pts',(1.50852499534242,-1.28458904017411,1.04188830921359));
#12803=CARTESIAN_POINT('Ctrl Pts',(0.473312455428654,-1.07028343020201,
1.04214267388586));
#12804=CARTESIAN_POINT('Ctrl Pts',(11.5121826600865,-1.26046981594517,1.0245894475956));
#12805=CARTESIAN_POINT('Ctrl Pts',(9.9393350416019,-1.42558521977072,1.02441268379886));
#12806=CARTESIAN_POINT('Ctrl Pts',(7.30818539134325,-1.64115782448209,1.02412850358181));
#12807=CARTESIAN_POINT('Ctrl Pts',(3.607597182252,-1.56868448653922,1.02422201615766));
#12808=CARTESIAN_POINT('Ctrl Pts',(1.50836811330665,-1.28557739750152,1.02462705425916));
#12809=CARTESIAN_POINT('Ctrl Pts',(0.473097162761967,-1.07132381406029,
1.02492790083044));
#12810=CARTESIAN_POINT('',(0.489277774073836,-0.993132359214002,1.1));
#12811=CARTESIAN_POINT('',(0.473097162761967,-1.07132381406029,1.02492790083044));
#12812=CARTESIAN_POINT('Origin',(0.489277774073836,-0.993132359214002,1.02));
#12813=CARTESIAN_POINT('Ctrl Pts',(0.473097162761967,-1.07132381406029,
1.02492790083044));
#12814=CARTESIAN_POINT('Ctrl Pts',(1.50836811330665,-1.28557739750152,1.02462705425916));
#12815=CARTESIAN_POINT('Ctrl Pts',(3.607597182252,-1.56868448653922,1.02422201615766));
#12816=CARTESIAN_POINT('Ctrl Pts',(7.30818539134325,-1.64115782448209,1.02412850358181));
#12817=CARTESIAN_POINT('Ctrl Pts',(9.9393350416019,-1.42558521977072,1.02441268379886));
#12818=CARTESIAN_POINT('Ctrl Pts',(11.5121826600865,-1.26046981594517,1.0245894475956));
#12819=CARTESIAN_POINT('Ctrl Pts',(11.5038445323836,-1.181038004955,1.1));
#12820=CARTESIAN_POINT('Ctrl Pts',(9.93221394244152,-1.34601544154236,1.1));
#12821=CARTESIAN_POINT('Ctrl Pts',(7.3047417451522,-1.56119993769491,1.1));
#12822=CARTESIAN_POINT('Ctrl Pts',(3.61332606662357,-1.48882378722464,1.1));
#12823=CARTESIAN_POINT('Ctrl Pts',(1.52093096174237,-1.20661833758759,1.1));
#12824=CARTESIAN_POINT('Ctrl Pts',(0.489277774073836,-0.993132359214002,
1.1));
#12825=CARTESIAN_POINT('Ctrl Pts',(0.489277774073836,-0.993132359214003,
1.1));
#12826=CARTESIAN_POINT('Ctrl Pts',(0.47591459116406,-0.990367038259462,
1.1));
#12827=CARTESIAN_POINT('Ctrl Pts',(0.446638556739065,-0.974524902741032,
1.1));
#12828=CARTESIAN_POINT('Ctrl Pts',(0.433565722548535,-0.942876078073176,
1.1));
#12829=CARTESIAN_POINT('Ctrl Pts',(0.433565722548535,-0.924681003894255,
1.1));
#12830=CARTESIAN_POINT('Ctrl Pts',(0.48461766586479,-1.01565194352286,1.1));
#12831=CARTESIAN_POINT('Ctrl Pts',(0.466871946563175,-1.01185427439077,
1.09999555360656));
#12832=CARTESIAN_POINT('Ctrl Pts',(0.428148998320346,-0.990723083341879,
1.0999884677795));
#12833=CARTESIAN_POINT('Ctrl Pts',(0.410637366989639,-0.948905017863894,
1.09999228132016));
#12834=CARTESIAN_POINT('Ctrl Pts',(0.410427643322096,-0.924681003894255,
1.1));
#12835=CARTESIAN_POINT('Ctrl Pts',(0.47653584926364,-1.05470664829667,1.08154627613271));
#12836=CARTESIAN_POINT('Ctrl Pts',(0.451238756159369,-1.04914377880765,
1.08175207965746));
#12837=CARTESIAN_POINT('Ctrl Pts',(0.396142217510869,-1.01881823177681,
1.08201099971769));
#12838=CARTESIAN_POINT('Ctrl Pts',(0.370857020273576,-0.959285462196374,
1.08165947596025));
#12839=CARTESIAN_POINT('Ctrl Pts',(0.370309350093454,-0.924681003894255,
1.0813056591965));
#12840=CARTESIAN_POINT('Ctrl Pts',(0.473312455428654,-1.07028343020201,
1.04214267388586));
#12841=CARTESIAN_POINT('Ctrl Pts',(0.444929265438756,-1.064235408557,1.04267704697817));
#12842=CARTESIAN_POINT('Ctrl Pts',(0.382898223041383,-1.03040761468413,
1.04335444671884));
#12843=CARTESIAN_POINT('Ctrl Pts',(0.354868227955524,-0.963393056722486,
1.04243119239046));
#12844=CARTESIAN_POINT('Ctrl Pts',(0.354583574894625,-0.924681003894255,
1.0415166534692));
#12845=CARTESIAN_POINT('Ctrl Pts',(0.473097162761967,-1.07132381406029,
1.02492790083044));
#12846=CARTESIAN_POINT('Ctrl Pts',(0.444494893732137,-1.06536514830602,
1.02555992378854));
#12847=CARTESIAN_POINT('Ctrl Pts',(0.381802689524125,-1.03137574421946,
1.02636429433614));
#12848=CARTESIAN_POINT('Ctrl Pts',(0.353731913874551,-0.963614141904928,
1.02526599313355));
#12849=CARTESIAN_POINT('Ctrl Pts',(0.35367535976817,-0.924681003894255,
1.02418687649944));
#12850=CARTESIAN_POINT('',(0.433565722548535,-0.924681003894255,1.1));
#12851=CARTESIAN_POINT('',(0.35367535976817,-0.924681003894255,1.02418687649944));
#12852=CARTESIAN_POINT('Origin',(0.433565722548536,-0.924681003894255,1.02));
#12853=CARTESIAN_POINT('Ctrl Pts',(0.35367535976817,-0.924681003894255,
1.02418687649944));
#12854=CARTESIAN_POINT('Ctrl Pts',(0.353731913874551,-0.963614141904928,
1.02526599313355));
#12855=CARTESIAN_POINT('Ctrl Pts',(0.381802689524125,-1.03137574421946,
1.02636429433614));
#12856=CARTESIAN_POINT('Ctrl Pts',(0.444494893732137,-1.06536514830602,
1.02555992378854));
#12857=CARTESIAN_POINT('Ctrl Pts',(0.473097162761967,-1.07132381406029,
1.02492790083044));
#12858=CARTESIAN_POINT('Ctrl Pts',(0.489277774073836,-0.993132359214003,
1.1));
#12859=CARTESIAN_POINT('Ctrl Pts',(0.47591459116406,-0.990367038259462,
1.1));
#12860=CARTESIAN_POINT('Ctrl Pts',(0.446638556739065,-0.974524902741032,
1.1));
#12861=CARTESIAN_POINT('Ctrl Pts',(0.433565722548535,-0.942876078073176,
1.1));
#12862=CARTESIAN_POINT('Ctrl Pts',(0.433565722548535,-0.924681003894255,
1.1));
#12863=CARTESIAN_POINT('Origin',(0.433565722548536,-0.526416499322631,1.02));
#12864=CARTESIAN_POINT('',(0.433565722548536,0.924681003894255,1.1));
#12865=CARTESIAN_POINT('',(0.35367535976817,0.924681003894255,1.02418687649944));
#12866=CARTESIAN_POINT('Origin',(0.433565722548536,0.924681003894255,1.02));
#12867=CARTESIAN_POINT('',(0.35367535976817,-0.526416499322631,1.02418687649944));
#12868=CARTESIAN_POINT('',(0.433565722548536,-0.526416499322631,1.1));
#12869=CARTESIAN_POINT('Ctrl Pts',(0.433565722548535,0.924681003894255,
1.1));
#12870=CARTESIAN_POINT('Ctrl Pts',(0.433565722548535,0.94287607801605,1.1));
#12871=CARTESIAN_POINT('Ctrl Pts',(0.44664012289244,0.97452669098104,1.1));
#12872=CARTESIAN_POINT('Ctrl Pts',(0.475914591206016,0.990367038268144,
1.1));
#12873=CARTESIAN_POINT('Ctrl Pts',(0.489277774073836,0.993132359214003,
1.1));
#12874=CARTESIAN_POINT('Ctrl Pts',(0.410427643322096,0.924681003894255,
1.1));
#12875=CARTESIAN_POINT('Ctrl Pts',(0.410637366988981,0.948905017787839,
1.09999228132018));
#12876=CARTESIAN_POINT('Ctrl Pts',(0.428151078432557,0.99072545440496,1.09998846767325));
#12877=CARTESIAN_POINT('Ctrl Pts',(0.466871946618891,1.01185427440269,1.09999555360657));
#12878=CARTESIAN_POINT('Ctrl Pts',(0.48461766586479,1.01565194352286,1.1));
#12879=CARTESIAN_POINT('Ctrl Pts',(0.370309350093454,0.924681003894255,
1.0813056591965));
#12880=CARTESIAN_POINT('Ctrl Pts',(0.370857020271857,0.959285462087728,
1.08165947595914));
#12881=CARTESIAN_POINT('Ctrl Pts',(0.396145183504025,1.01882160767722,1.08201100382378));
#12882=CARTESIAN_POINT('Ctrl Pts',(0.451238756238795,1.04914377882512,1.08175207965681));
#12883=CARTESIAN_POINT('Ctrl Pts',(0.47653584926364,1.05470664829667,1.08154627613271));
#12884=CARTESIAN_POINT('Ctrl Pts',(0.354583574894625,0.924681003894255,
1.0415166534692));
#12885=CARTESIAN_POINT('Ctrl Pts',(0.35486822795463,0.963393056600943,1.04243119238759));
#12886=CARTESIAN_POINT('Ctrl Pts',(0.382901552879886,1.03041141096935,1.04335445746542));
#12887=CARTESIAN_POINT('Ctrl Pts',(0.444929265527871,1.06423540857599,1.04267704697649));
#12888=CARTESIAN_POINT('Ctrl Pts',(0.473312455428654,1.07028343020201,1.04214267388586));
#12889=CARTESIAN_POINT('Ctrl Pts',(0.35367535976817,0.924681003894255,1.02418687649944));
#12890=CARTESIAN_POINT('Ctrl Pts',(0.353731913874373,0.963614141782691,
1.02526599313016));
#12891=CARTESIAN_POINT('Ctrl Pts',(0.381806046235973,1.03137957549636,1.02636430709951));
#12892=CARTESIAN_POINT('Ctrl Pts',(0.44449489382194,1.06536514832473,1.02555992378656));
#12893=CARTESIAN_POINT('Ctrl Pts',(0.473097162761967,1.07132381406029,1.02492790083044));
#12894=CARTESIAN_POINT('',(0.489277774073836,0.993132359214003,1.1));
#12895=CARTESIAN_POINT('',(0.473097162761967,1.07132381406029,1.02492790083044));
#12896=CARTESIAN_POINT('Origin',(0.489277774073836,0.993132359214003,1.02));
#12897=CARTESIAN_POINT('Ctrl Pts',(0.473097162761967,1.07132381406029,1.02492790083044));
#12898=CARTESIAN_POINT('Ctrl Pts',(0.44449489382194,1.06536514832473,1.02555992378656));
#12899=CARTESIAN_POINT('Ctrl Pts',(0.381806046235973,1.03137957549636,1.02636430709951));
#12900=CARTESIAN_POINT('Ctrl Pts',(0.353731913874373,0.963614141782691,
1.02526599313016));
#12901=CARTESIAN_POINT('Ctrl Pts',(0.35367535976817,0.924681003894255,1.02418687649944));
#12902=CARTESIAN_POINT('Ctrl Pts',(0.433565722548535,0.924681003894255,
1.1));
#12903=CARTESIAN_POINT('Ctrl Pts',(0.433565722548535,0.94287607801605,1.1));
#12904=CARTESIAN_POINT('Ctrl Pts',(0.44664012289244,0.97452669098104,1.1));
#12905=CARTESIAN_POINT('Ctrl Pts',(0.475914591206016,0.990367038268144,
1.1));
#12906=CARTESIAN_POINT('Ctrl Pts',(0.489277774073836,0.993132359214003,
1.1));
#12907=CARTESIAN_POINT('Ctrl Pts',(0.489277774073836,0.993132359214003,
1.1));
#12908=CARTESIAN_POINT('Ctrl Pts',(1.52092917355268,1.20661796754713,1.1));
#12909=CARTESIAN_POINT('Ctrl Pts',(3.61335021200387,1.48882484395407,1.1));
#12910=CARTESIAN_POINT('Ctrl Pts',(7.30471495328446,1.56119985233321,1.1));
#12911=CARTESIAN_POINT('Ctrl Pts',(9.93221666658724,1.34601515558293,1.1));
#12912=CARTESIAN_POINT('Ctrl Pts',(11.5038445323836,1.18103800495499,1.1));
#12913=CARTESIAN_POINT('Ctrl Pts',(0.48461766586479,1.01565194352286,1.1));
#12914=CARTESIAN_POINT('Ctrl Pts',(1.51730408437175,1.22941144654908,1.10000211650524));
#12915=CARTESIAN_POINT('Ctrl Pts',(3.61168692820091,1.5119477834436,1.09999968963693));
#12916=CARTESIAN_POINT('Ctrl Pts',(7.30571671988008,1.58436788793099,1.10000007151498));
#12917=CARTESIAN_POINT('Ctrl Pts',(9.9342747920155,1.36902164623626,1.10000125302125));
#12918=CARTESIAN_POINT('Ctrl Pts',(11.5062520964801,1.2039732708886,1.1));
#12919=CARTESIAN_POINT('Ctrl Pts',(0.476539293980872,1.05469000198791,1.08153107638517));
#12920=CARTESIAN_POINT('Ctrl Pts',(1.51100975601983,1.26891510265927,1.08143311289086));
#12921=CARTESIAN_POINT('Ctrl Pts',(3.60881166804804,1.5520238347382,1.08130174382265));
#12922=CARTESIAN_POINT('Ctrl Pts',(7.30744439783659,1.62451931411139,1.08127113658549));
#12923=CARTESIAN_POINT('Ctrl Pts',(9.9378457243824,1.40889498800017,1.08136351985702));
#12924=CARTESIAN_POINT('Ctrl Pts',(11.5104252017938,1.24372767671385,1.08142125970198));
#12925=CARTESIAN_POINT('Ctrl Pts',(0.473312455428654,1.07028343020201,1.04214267388586));
#12926=CARTESIAN_POINT('Ctrl Pts',(1.50852320098322,1.28458866871296,1.04188830965449));
#12927=CARTESIAN_POINT('Ctrl Pts',(3.60768294746331,1.5677700397583,1.04154645950336));
#12928=CARTESIAN_POINT('Ctrl Pts',(7.30812316513016,1.64026109291585,1.04146726882447));
#12929=CARTESIAN_POINT('Ctrl Pts',(9.93925233633459,1.42463352276678,1.04170731205607));
#12930=CARTESIAN_POINT('Ctrl Pts',(11.5120790720622,1.25948300155991,1.0418569252725));
#12931=CARTESIAN_POINT('Ctrl Pts',(0.473097162761967,1.07132381406029,1.02492790083044));
#12932=CARTESIAN_POINT('Ctrl Pts',(1.50836631884621,1.28557702613055,1.02462705478063));
#12933=CARTESIAN_POINT('Ctrl Pts',(3.60762138890097,1.56868554702656,1.02422201460129));
#12934=CARTESIAN_POINT('Ctrl Pts',(7.30815854116978,1.64115773776738,1.02412850382783));
#12935=CARTESIAN_POINT('Ctrl Pts',(9.93933776785713,1.42558493357216,1.02441268410525));
#12936=CARTESIAN_POINT('Ctrl Pts',(11.5121826600865,1.26046981594517,1.0245894475956));
#12937=CARTESIAN_POINT('Ctrl Pts',(11.5121826600865,1.26046981594517,1.0245894475956));
#12938=CARTESIAN_POINT('Ctrl Pts',(9.93933776785713,1.42558493357216,1.02441268410525));
#12939=CARTESIAN_POINT('Ctrl Pts',(7.30815854116978,1.64115773776738,1.02412850382783));
#12940=CARTESIAN_POINT('Ctrl Pts',(3.60762138890097,1.56868554702656,1.02422201460129));
#12941=CARTESIAN_POINT('Ctrl Pts',(1.50836631884621,1.28557702613055,1.02462705478063));
#12942=CARTESIAN_POINT('Ctrl Pts',(0.473097162761967,1.07132381406029,1.02492790083044));
#12943=CARTESIAN_POINT('Ctrl Pts',(0.489277774073836,0.993132359214003,
1.1));
#12944=CARTESIAN_POINT('Ctrl Pts',(1.52092917355268,1.20661796754713,1.1));
#12945=CARTESIAN_POINT('Ctrl Pts',(3.61335021200387,1.48882484395407,1.1));
#12946=CARTESIAN_POINT('Ctrl Pts',(7.30471495328446,1.56119985233321,1.1));
#12947=CARTESIAN_POINT('Ctrl Pts',(9.93221666658724,1.34601515558293,1.1));
#12948=CARTESIAN_POINT('Ctrl Pts',(11.5038445323836,1.18103800495499,1.1));
#12949=CARTESIAN_POINT('Origin',(0.347167001354737,-1.05283299864526,0.9));
#12950=CARTESIAN_POINT('',(0.347167001354737,0.931160914046453,0.9));
#12951=CARTESIAN_POINT('Ctrl Pts',(0.347167001354737,0.931160914046453,
0.9));
#12952=CARTESIAN_POINT('Ctrl Pts',(0.34933645413337,0.929000934518636,0.941395625006663));
#12953=CARTESIAN_POINT('Ctrl Pts',(0.351505906937822,0.926840964458487,
0.982791250505987));
#12954=CARTESIAN_POINT('Ctrl Pts',(0.35367535976817,0.924681003894255,1.02418687649944));
#12955=CARTESIAN_POINT('',(0.347167001354737,-0.931160914046453,0.9));
#12956=CARTESIAN_POINT('',(0.347167001354737,-1.05283299864526,0.9));
#12957=CARTESIAN_POINT('Ctrl Pts',(0.35367535976817,-0.924681003894255,
1.02418687649944));
#12958=CARTESIAN_POINT('Ctrl Pts',(0.351505906937822,-0.926840964458487,
0.982791250505987));
#12959=CARTESIAN_POINT('Ctrl Pts',(0.34933645413337,-0.929000934518636,
0.941395625006663));
#12960=CARTESIAN_POINT('Ctrl Pts',(0.347167001354737,-0.931160914046453,
0.9));
#12961=CARTESIAN_POINT('Ctrl Pts',(0.346994979645257,0.93133218461645,0.89671763024815));
#12962=CARTESIAN_POINT('Ctrl Pts',(0.349221772992334,0.929115114391563,
0.939207378479044));
#12963=CARTESIAN_POINT('Ctrl Pts',(0.35144856636661,0.926898054140648,0.981697127228945));
#12964=CARTESIAN_POINT('Ctrl Pts',(0.35367535976817,0.924681003894255,1.02418687649944));
#12965=CARTESIAN_POINT('Ctrl Pts',(0.347101141748081,0.970260862175626,
0.898743323843195));
#12966=CARTESIAN_POINT('Ctrl Pts',(0.349327989245423,0.968041585482289,
0.94123294798136));
#12967=CARTESIAN_POINT('Ctrl Pts',(0.35155465541633,0.96582239703375,0.983722586263841));
#12968=CARTESIAN_POINT('Ctrl Pts',(0.353781503060223,0.96360313540272,1.02621221116359));
#12969=CARTESIAN_POINT('Ctrl Pts',(0.375231247034764,1.03797686888013,0.90080243726586));
#12970=CARTESIAN_POINT('Ctrl Pts',(0.377454726329371,1.03575393200526,0.943292036336267));
#12971=CARTESIAN_POINT('Ctrl Pts',(0.379678256934949,1.03353096064141,0.985781630873016));
#12972=CARTESIAN_POINT('Ctrl Pts',(0.381901729528225,1.03130803054038,1.02827123060239));
#12973=CARTESIAN_POINT('Ctrl Pts',(0.437891832981715,1.07196344732884,0.899291918906528));
#12974=CARTESIAN_POINT('Ctrl Pts',(0.440109459023804,1.06974216787274,0.941781905864285));
#12975=CARTESIAN_POINT('Ctrl Pts',(0.442327107866739,1.06752094195844,0.984271894420663));
#12976=CARTESIAN_POINT('Ctrl Pts',(0.44454471435444,1.06529967134173,1.02676188280081));
#12977=CARTESIAN_POINT('Ctrl Pts',(0.466484255634356,1.07794817238022,0.898105730168711));
#12978=CARTESIAN_POINT('Ctrl Pts',(0.46869984010673,1.07572875745303,0.940595920481163));
#12979=CARTESIAN_POINT('Ctrl Pts',(0.470915412358444,1.07350934859911,0.983086111716909));
#12980=CARTESIAN_POINT('Ctrl Pts',(0.473130972350001,1.07128994583173,1.02557630387858));
#12981=CARTESIAN_POINT('',(0.466583029361855,1.07784922788182,0.9));
#12982=CARTESIAN_POINT('Ctrl Pts',(0.473097162761967,1.07132381406029,1.02492790083044));
#12983=CARTESIAN_POINT('Ctrl Pts',(0.470925796725269,1.07349894615889,0.983285266331776));
#12984=CARTESIAN_POINT('Ctrl Pts',(0.468754418912838,1.07567408410356,0.941642632722456));
#12985=CARTESIAN_POINT('Ctrl Pts',(0.466583029361855,1.07784922788182,0.9));
#12986=CARTESIAN_POINT('Ctrl Pts',(0.466583029361856,1.07784922788182,0.9));
#12987=CARTESIAN_POINT('Ctrl Pts',(0.45605169130101,1.07567238924625,0.899999999995368));
#12988=CARTESIAN_POINT('Ctrl Pts',(0.445810809951917,1.07234818111891,0.899998625774342));
#12989=CARTESIAN_POINT('Ctrl Pts',(0.436024610942277,1.06798890472683,0.899998407511246));
#12990=CARTESIAN_POINT('Ctrl Pts',(0.42804650025127,1.0644350438709,0.899998229574221));
#12991=CARTESIAN_POINT('Ctrl Pts',(0.420370119207661,1.06019193848671,0.899998775177391));
#12992=CARTESIAN_POINT('Ctrl Pts',(0.413095080427888,1.05529723033767,0.89999964722522));
#12993=CARTESIAN_POINT('Ctrl Pts',(0.404948343152914,1.04981603600524,0.900000623762221));
#12994=CARTESIAN_POINT('Ctrl Pts',(0.3973835293994,1.04357129238854,0.900002055204145));
#12995=CARTESIAN_POINT('Ctrl Pts',(0.390528747317286,1.03663323920468,0.900000884971142));
#12996=CARTESIAN_POINT('Ctrl Pts',(0.38377850537204,1.02980099609921,0.899999732584995));
#12997=CARTESIAN_POINT('Ctrl Pts',(0.377716121663402,1.02229558340178,0.899996048870533));
#12998=CARTESIAN_POINT('Ctrl Pts',(0.372394770625083,1.01423711207676,0.899993306941804));
#12999=CARTESIAN_POINT('Ctrl Pts',(0.366459905306112,1.00524955578769,0.899990248888012));
#13000=CARTESIAN_POINT('Ctrl Pts',(0.361501411166698,0.995658501454654,
0.8999884459165));
#13001=CARTESIAN_POINT('Ctrl Pts',(0.35758177265536,0.985639755107121,0.899989063766683));
#13002=CARTESIAN_POINT('Ctrl Pts',(0.356156017388132,0.981995469968403,
0.8999892885076));
#13003=CARTESIAN_POINT('Ctrl Pts',(0.354868143601992,0.978294337124559,
0.899989797558581));
#13004=CARTESIAN_POINT('Ctrl Pts',(0.353722739999278,0.97454418014098,0.899990530873797));
#13005=CARTESIAN_POINT('Ctrl Pts',(0.350595356382139,0.964304837882626,
0.899992533100777));
#13006=CARTESIAN_POINT('Ctrl Pts',(0.348551371116014,0.953782216732967,
0.899996407005639));
#13007=CARTESIAN_POINT('Ctrl Pts',(0.347666342074759,0.943140644221274,
0.899998614621972));
#13008=CARTESIAN_POINT('Ctrl Pts',(0.347335396628921,0.939161362417926,
0.899999440132251));
#13009=CARTESIAN_POINT('Ctrl Pts',(0.347167001797138,0.935165318330998,
0.899999999966431));
#13010=CARTESIAN_POINT('Ctrl Pts',(0.347167001354737,0.931160914046453,
0.9));
#13011=CARTESIAN_POINT('Ctrl Pts',(0.466583029361855,1.07784922788182,0.9));
#13012=CARTESIAN_POINT('Ctrl Pts',(0.468719324182819,1.07566682993082,0.941642633610146));
#13013=CARTESIAN_POINT('Ctrl Pts',(0.470855619003782,1.07348443197981,0.983285267220292));
#13014=CARTESIAN_POINT('Ctrl Pts',(0.472991913824746,1.07130203402881,1.02492790083044));
#13015=CARTESIAN_POINT('Ctrl Pts',(4.1506201585889,1.83934349355009,0.9));
#13016=CARTESIAN_POINT('Ctrl Pts',(4.15133415151554,1.83716109559909,0.941642633610146));
#13017=CARTESIAN_POINT('Ctrl Pts',(4.15204814444219,1.83497869764808,0.983285267220293));
#13018=CARTESIAN_POINT('Ctrl Pts',(4.15276213736883,1.83279629969708,1.02492790083044));
#13019=CARTESIAN_POINT('Ctrl Pts',(7.83465728781595,1.65326443611903,0.9));
#13020=CARTESIAN_POINT('Ctrl Pts',(7.83394897884827,1.65108203816803,0.941642633610146));
#13021=CARTESIAN_POINT('Ctrl Pts',(7.83324066988059,1.64889964021702,0.983285267220292));
#13022=CARTESIAN_POINT('Ctrl Pts',(7.83253236091292,1.64671724226602,1.02492790083044));
#13023=CARTESIAN_POINT('Ctrl Pts',(11.518694417043,1.26698486563531,0.9));
#13024=CARTESIAN_POINT('Ctrl Pts',(11.516563806181,1.26480246768431,0.941642633610146));
#13025=CARTESIAN_POINT('Ctrl Pts',(11.514433195319,1.2626200697333,0.983285267220292));
#13026=CARTESIAN_POINT('Ctrl Pts',(11.512302584457,1.2604376717823,1.02492790083044));
#13027=CARTESIAN_POINT('',(11.518694417043,1.26698486563531,0.9));
#13028=CARTESIAN_POINT('Ctrl Pts',(11.518694417043,1.26698486563531,0.9));
#13029=CARTESIAN_POINT('Ctrl Pts',(11.5165238247878,1.26481317761477,0.941529815291285));
#13030=CARTESIAN_POINT('Ctrl Pts',(11.5143532391283,1.26264149437998,0.983059631155884));
#13031=CARTESIAN_POINT('Ctrl Pts',(11.5121826600865,1.26046981594516,1.0245894475956));
#13032=CARTESIAN_POINT('Ctrl Pts',(0.466583029361855,1.07784922788182,0.9));
#13033=CARTESIAN_POINT('Ctrl Pts',(4.1506201585889,1.83934349355009,0.9));
#13034=CARTESIAN_POINT('Ctrl Pts',(7.83465728781595,1.65326443611903,0.9));
#13035=CARTESIAN_POINT('Ctrl Pts',(11.518694417043,1.26698486563531,0.9));
#13036=CARTESIAN_POINT('Ctrl Pts',(11.5188237574534,1.26711427133763,0.897525337604991));
#13037=CARTESIAN_POINT('Ctrl Pts',(11.5166039145442,1.26489330787379,0.939997457644392));
#13038=CARTESIAN_POINT('Ctrl Pts',(11.5143840785328,1.26267234941507,0.982469578283382));
#13039=CARTESIAN_POINT('Ctrl Pts',(11.512164249443,1.26045139597664,1.02494169952389));
#13040=CARTESIAN_POINT('Ctrl Pts',(11.560356924166,1.2626472646828,0.899468475190601));
#13041=CARTESIAN_POINT('Ctrl Pts',(11.5581357517162,1.26042470505353,0.941940442504879));
#13042=CARTESIAN_POINT('Ctrl Pts',(11.5559146107476,1.25820228015812,0.984412418590584));
#13043=CARTESIAN_POINT('Ctrl Pts',(11.5536934488601,1.25597972716877,1.02688438676053));
#13044=CARTESIAN_POINT('Ctrl Pts',(11.6290545561482,1.22266466287338,0.9009785794625));
#13045=CARTESIAN_POINT('Ctrl Pts',(11.6268300646776,1.22044146949289,0.943450343593379));
#13046=CARTESIAN_POINT('Ctrl Pts',(11.6246055668724,1.21821824717544,0.985922105839347));
#13047=CARTESIAN_POINT('Ctrl Pts',(11.6223810783988,1.21599505938238,1.02839387038768));
#13048=CARTESIAN_POINT('Ctrl Pts',(11.652916631058,1.14949843694546,0.898404198500408));
#13049=CARTESIAN_POINT('Ctrl Pts',(11.6506907663731,1.14727726203421,0.940876003223652));
#13050=CARTESIAN_POINT('Ctrl Pts',(11.6484649368037,1.14505607393729,0.9833478090785));
#13051=CARTESIAN_POINT('Ctrl Pts',(11.6462390720682,1.14283490928962,1.02581961432614));
#13052=CARTESIAN_POINT('Ctrl Pts',(11.6530022067803,1.11817769023529,0.896771316447588));
#13053=CARTESIAN_POINT('Ctrl Pts',(11.6507763512808,1.11595737261641,0.939243169479033));
#13054=CARTESIAN_POINT('Ctrl Pts',(11.6485504957647,1.11373706111287,0.981715022829298));
#13055=CARTESIAN_POINT('Ctrl Pts',(11.6463246402318,1.11151675574496,1.02418687649944));
#13056=CARTESIAN_POINT('',(11.6528329986453,1.11800890309831,0.9));
#13057=CARTESIAN_POINT('Ctrl Pts',(11.6463246402318,1.11151675574496,1.02418687649944));
#13058=CARTESIAN_POINT('Ctrl Pts',(11.6484940930522,1.11368079904038,0.982791250696082));
#13059=CARTESIAN_POINT('Ctrl Pts',(11.6506635458567,1.11584484816443,0.941395625196594));
#13060=CARTESIAN_POINT('Ctrl Pts',(11.6528329986453,1.11800890309831,0.9));
#13061=CARTESIAN_POINT('Ctrl Pts',(11.6528329986453,1.11800890309831,0.9));
#13062=CARTESIAN_POINT('Ctrl Pts',(11.6528329983633,1.12876627611802,0.899999999993021));
#13063=CARTESIAN_POINT('Ctrl Pts',(11.6516446702457,1.13947128553817,0.899998527904116));
#13064=CARTESIAN_POINT('Ctrl Pts',(11.6493511293179,1.14994150848088,0.899998119066462));
#13065=CARTESIAN_POINT('Ctrl Pts',(11.6474764306251,1.15849967852608,0.89999778488999));
#13066=CARTESIAN_POINT('Ctrl Pts',(11.6448621032167,1.16690170462481,0.899998134702192));
#13067=CARTESIAN_POINT('Ctrl Pts',(11.6415284502961,1.17504213011111,0.899998933310541));
#13068=CARTESIAN_POINT('Ctrl Pts',(11.6374537398456,1.18499213918264,0.899999909446287));
#13069=CARTESIAN_POINT('Ctrl Pts',(11.6323486952005,1.19444663470912,0.900001674548864));
#13070=CARTESIAN_POINT('Ctrl Pts',(11.6262733681268,1.20322237541324,0.900000560254235));
#13071=CARTESIAN_POINT('Ctrl Pts',(11.6256011619285,1.20419336960417,0.900000436962806));
#13072=CARTESIAN_POINT('Ctrl Pts',(11.6249170295004,1.20515603220147,0.900000274771288));
#13073=CARTESIAN_POINT('Ctrl Pts',(11.6242210175348,1.20611009565643,0.900000065883751));
#13074=CARTESIAN_POINT('Ctrl Pts',(11.6197944794931,1.21217780481426,0.899998737388448));
#13075=CARTESIAN_POINT('Ctrl Pts',(11.6148881172219,1.21789846943619,0.899995595976687));
#13076=CARTESIAN_POINT('Ctrl Pts',(11.6095544776251,1.22323873890669,0.899992615091414));
#13077=CARTESIAN_POINT('Ctrl Pts',(11.601940589012,1.23086209181126,0.899988359811689));
#13078=CARTESIAN_POINT('Ctrl Pts',(11.5935341028624,1.23763544449334,0.899984652834703));
#13079=CARTESIAN_POINT('Ctrl Pts',(11.584505756877,1.24347857204465,0.899983891616646));
#13080=CARTESIAN_POINT('Ctrl Pts',(11.5791642013329,1.24693561616068,0.899983441247493));
#13081=CARTESIAN_POINT('Ctrl Pts',(11.5736041411459,1.25006639925598,0.89998394495257));
#13082=CARTESIAN_POINT('Ctrl Pts',(11.5678562300951,1.25284717822614,0.899985279956182));
#13083=CARTESIAN_POINT('Ctrl Pts',(11.5582100984591,1.25751387535486,0.899987520356298));
#13084=CARTESIAN_POINT('Ctrl Pts',(11.548125859505,1.26115381593413,0.899992245475585));
#13085=CARTESIAN_POINT('Ctrl Pts',(11.5377575652696,1.26367454383615,0.899995957332528));
#13086=CARTESIAN_POINT('Ctrl Pts',(11.5314967650479,1.26519666246525,0.899998198703601));
#13087=CARTESIAN_POINT('Ctrl Pts',(11.5251318445822,1.26630988651457,0.89999999997641));
#13088=CARTESIAN_POINT('Ctrl Pts',(11.518694417043,1.26698486563531,0.900000000000001));
#13089=CARTESIAN_POINT('Origin',(6.0828528088686,0.,1.1));
#13090=CARTESIAN_POINT('Origin',(11.6528329986453,1.25283299864526,0.9));
#13091=CARTESIAN_POINT('',(11.6528329986453,-1.11800890309831,0.9));
#13092=CARTESIAN_POINT('Ctrl Pts',(11.6528329986453,-1.11800890309831,0.9));
#13093=CARTESIAN_POINT('Ctrl Pts',(11.6506635458567,-1.11584484816443,0.941395625196595));
#13094=CARTESIAN_POINT('Ctrl Pts',(11.6484940930522,-1.11368079904038,0.98279125069608));
#13095=CARTESIAN_POINT('Ctrl Pts',(11.6463246402318,-1.11151675574497,1.02418687649944));
#13096=CARTESIAN_POINT('',(11.6528329986453,1.25283299864526,0.9));
#13097=CARTESIAN_POINT('Ctrl Pts',(0.466487690105381,-1.07794473197144,
0.898171596006697));
#13098=CARTESIAN_POINT('Ctrl Pts',(0.468702129741454,-1.07572646385346,
0.940639831040774));
#13099=CARTESIAN_POINT('Ctrl Pts',(0.470916557169473,-1.07350820180247,
0.983108066997194));
#13100=CARTESIAN_POINT('Ctrl Pts',(0.473130972350001,-1.07128994583173,
1.02557630387858));
#13101=CARTESIAN_POINT('Ctrl Pts',(0.428364464143914,-1.0699650947497,0.899753180570758));
#13102=CARTESIAN_POINT('Ctrl Pts',(0.430581658228805,-1.06774429850715,
0.942221140547455));
#13103=CARTESIAN_POINT('Ctrl Pts',(0.432798785432897,-1.06552370176641,
0.98468911452651));
#13104=CARTESIAN_POINT('Ctrl Pts',(0.435015961689253,-1.0633029131784,1.02715707577488));
#13105=CARTESIAN_POINT('Ctrl Pts',(0.367703220512368,-1.02873213740117,
0.900780809445176));
#13106=CARTESIAN_POINT('Ctrl Pts',(0.369926480243704,-1.02651076835199,
0.943248428164859));
#13107=CARTESIAN_POINT('Ctrl Pts',(0.372149767842394,-1.02428934262989,
0.985716042409561));
#13108=CARTESIAN_POINT('Ctrl Pts',(0.374373022752712,-1.02206798136513,
1.0281836617465));
#13109=CARTESIAN_POINT('Ctrl Pts',(0.347078053061478,-0.96052525347768,
0.898302765458188));
#13110=CARTESIAN_POINT('Ctrl Pts',(0.349303707759805,-0.958307704298137,
0.940770468670701));
#13111=CARTESIAN_POINT('Ctrl Pts',(0.351529312469145,-0.956090135383351,
0.983238173449507));
#13112=CARTESIAN_POINT('Ctrl Pts',(0.35375496723721,-0.953872602525604,
1.02570587749755));
#13113=CARTESIAN_POINT('Ctrl Pts',(0.346998431491642,-0.931328747842296,
0.896783495400846));
#13114=CARTESIAN_POINT('Ctrl Pts',(0.349224074223285,-0.929112823219098,
0.939251288581378));
#13115=CARTESIAN_POINT('Ctrl Pts',(0.3514497169821,-0.926896908559584,0.98171908228038));
#13116=CARTESIAN_POINT('Ctrl Pts',(0.35367535976817,-0.924681003894255,
1.02418687649944));
#13117=CARTESIAN_POINT('',(0.466583029361856,-1.07784922788182,0.9));
#13118=CARTESIAN_POINT('Ctrl Pts',(0.347167001354737,-0.931160914046453,
0.9));
#13119=CARTESIAN_POINT('Ctrl Pts',(0.34716700178392,-0.941918922633709,
0.89999999999014));
#13120=CARTESIAN_POINT('Ctrl Pts',(0.348348457226296,-0.952625037179515,
0.899998920330619));
#13121=CARTESIAN_POINT('Ctrl Pts',(0.350635026118381,-0.963095666025449,
0.899998881610567));
#13122=CARTESIAN_POINT('Ctrl Pts',(0.352503737518513,-0.971652846855939,
0.899998849966385));
#13123=CARTESIAN_POINT('Ctrl Pts',(0.355111758040853,-0.980053468583104,
0.899999488623984));
#13124=CARTESIAN_POINT('Ctrl Pts',(0.358442500181925,-0.988191468018609,
0.900000335306729));
#13125=CARTESIAN_POINT('Ctrl Pts',(0.362154764014137,-0.997261639077022,
0.900001278973215));
#13126=CARTESIAN_POINT('Ctrl Pts',(0.366728534310471,-1.00591832418384,
0.900002536038328));
#13127=CARTESIAN_POINT('Ctrl Pts',(0.372121756320194,-1.01402249383533,
0.900001139180886));
#13128=CARTESIAN_POINT('Ctrl Pts',(0.377460617198322,-1.02204497728291,
0.899999756403108));
#13129=CARTESIAN_POINT('Ctrl Pts',(0.383603173789776,-1.02952688289601,
0.899995781932517));
#13130=CARTESIAN_POINT('Ctrl Pts',(0.390441954151244,-1.03639066990207,
0.899992822880961));
#13131=CARTESIAN_POINT('Ctrl Pts',(0.398043576670582,-1.0440200884702,0.899989533757499));
#13132=CARTESIAN_POINT('Ctrl Pts',(0.406433719974705,-1.0508151602132,0.89998759991803));
#13133=CARTESIAN_POINT('Ctrl Pts',(0.415453314813275,-1.05667842789903,
0.899988256654353));
#13134=CARTESIAN_POINT('Ctrl Pts',(0.418717986328798,-1.05880065659603,
0.899988494362188));
#13135=CARTESIAN_POINT('Ctrl Pts',(0.422065457324696,-1.0608004431648,0.89998903479261));
#13136=CARTESIAN_POINT('Ctrl Pts',(0.425489105966494,-1.06267176343868,
0.899989815051126));
#13137=CARTESIAN_POINT('Ctrl Pts',(0.434878177994434,-1.06780370385578,
0.899991954845297));
#13138=CARTESIAN_POINT('Ctrl Pts',(0.444763746614507,-1.07193185662919,
0.899996125260102));
#13139=CARTESIAN_POINT('Ctrl Pts',(0.455000483828058,-1.07494865668414,
0.899998508040168));
#13140=CARTESIAN_POINT('Ctrl Pts',(0.458814676066972,-1.07607271165555,
0.899999395860286));
#13141=CARTESIAN_POINT('Ctrl Pts',(0.462677844602733,-1.07704202188211,
0.899999999981245));
#13142=CARTESIAN_POINT('Ctrl Pts',(0.466583029361856,-1.07784922788182,
0.9));
#13143=CARTESIAN_POINT('Ctrl Pts',(0.466583029361855,-1.07784922788182,
0.9));
#13144=CARTESIAN_POINT('Ctrl Pts',(0.468754418912838,-1.07567408410356,
0.941642632722455));
#13145=CARTESIAN_POINT('Ctrl Pts',(0.470925796725269,-1.07349894615889,
0.983285266331777));
#13146=CARTESIAN_POINT('Ctrl Pts',(0.473097162761967,-1.07132381406029,
1.02492790083044));
#13147=CARTESIAN_POINT('Ctrl Pts',(11.6530064742455,-1.11818194708322,0.896689888359234));
#13148=CARTESIAN_POINT('Ctrl Pts',(11.6507791962577,-1.11596021050721,0.93918888408639));
#13149=CARTESIAN_POINT('Ctrl Pts',(11.6485519182532,-1.11373848005435,0.98168788013277));
#13150=CARTESIAN_POINT('Ctrl Pts',(11.6463246402318,-1.11151675574497,1.02418687649944));
#13151=CARTESIAN_POINT('Ctrl Pts',(11.6528923732761,-1.15994294490385,0.898867064552409));
#13152=CARTESIAN_POINT('Ctrl Pts',(11.6506650597175,-1.15772003758575,0.94136599317676));
#13153=CARTESIAN_POINT('Ctrl Pts',(11.6484378630123,-1.15549719156343,0.98386493116262));
#13154=CARTESIAN_POINT('Ctrl Pts',(11.646210549347,-1.15327429380451,1.02636386026838));
#13155=CARTESIAN_POINT('Ctrl Pts',(11.6202781937939,-1.23241532269502,0.900946494593638));
#13156=CARTESIAN_POINT('Ctrl Pts',(11.6180528194216,-1.23019050716461,0.943445418126786));
#13157=CARTESIAN_POINT('Ctrl Pts',(11.61582741935,-1.22796567893144,0.985944339620759));
#13158=CARTESIAN_POINT('Ctrl Pts',(11.6136020491686,-1.22574086850162,1.02844326360542));
#13159=CARTESIAN_POINT('Ctrl Pts',(11.5499778903249,-1.26376827666489,0.89890126240954));
#13160=CARTESIAN_POINT('Ctrl Pts',(11.5477556460229,-1.26154471817669,0.941400412665532));
#13161=CARTESIAN_POINT('Ctrl Pts',(11.5455333818837,-1.25932119531825,0.983899563748029));
#13162=CARTESIAN_POINT('Ctrl Pts',(11.5433111490058,-1.25709764437074,1.02639871495137));
#13163=CARTESIAN_POINT('Ctrl Pts',(11.5188280133912,-1.26711852942379,0.897443909004722));
#13164=CARTESIAN_POINT('Ctrl Pts',(11.5166067518272,-1.2648961465915,0.93994317191011));
#13165=CARTESIAN_POINT('Ctrl Pts',(11.5143854971699,-1.26267376877071,0.982442435415857));
#13166=CARTESIAN_POINT('Ctrl Pts',(11.512164249443,-1.26045139597664,1.02494169952389));
#13167=CARTESIAN_POINT('',(11.518694417043,-1.26698486563531,0.9));
#13168=CARTESIAN_POINT('Ctrl Pts',(11.5121826600865,-1.26046981594517,1.02458944759559));
#13169=CARTESIAN_POINT('Ctrl Pts',(11.5143532391283,-1.26264149437998,0.983059631155874));
#13170=CARTESIAN_POINT('Ctrl Pts',(11.5165238247878,-1.26481317761477,0.941529815291278));
#13171=CARTESIAN_POINT('Ctrl Pts',(11.518694417043,-1.26698486563531,0.900000000000001));
#13172=CARTESIAN_POINT('Ctrl Pts',(11.518694417043,-1.26698486563531,0.9));
#13173=CARTESIAN_POINT('Ctrl Pts',(11.5293907449245,-1.26586333143554,0.89999999999772));
#13174=CARTESIAN_POINT('Ctrl Pts',(11.5399108669542,-1.26356499290392,0.899998338215302));
#13175=CARTESIAN_POINT('Ctrl Pts',(11.5500820708623,-1.26019169516113,0.899997799246518));
#13176=CARTESIAN_POINT('Ctrl Pts',(11.5583854467913,-1.257437865867,0.899997359253331));
#13177=CARTESIAN_POINT('Ctrl Pts',(11.5664568733073,-1.25396634382171,0.899997630752438));
#13178=CARTESIAN_POINT('Ctrl Pts',(11.5741940388996,-1.24980829733595,0.899998424072895));
#13179=CARTESIAN_POINT('Ctrl Pts',(11.5836658766397,-1.2447180170313,0.899999395255759));
#13180=CARTESIAN_POINT('Ctrl Pts',(11.5925370694996,-1.23865400393036,0.900001263097414));
#13181=CARTESIAN_POINT('Ctrl Pts',(11.6006317325417,-1.23169548876955,0.900000312360774));
#13182=CARTESIAN_POINT('Ctrl Pts',(11.6015335603822,-1.23092023936527,0.900000206439036));
#13183=CARTESIAN_POINT('Ctrl Pts',(11.602425722662,-1.23013384139825,0.900000061718141));
#13184=CARTESIAN_POINT('Ctrl Pts',(11.6033079529217,-1.22933637123764,0.899999870107331));
#13185=CARTESIAN_POINT('Ctrl Pts',(11.6088666967428,-1.22431168263841,0.899998662808674));
#13186=CARTESIAN_POINT('Ctrl Pts',(11.6140319692072,-1.21884801843051,0.89999566823453));
#13187=CARTESIAN_POINT('Ctrl Pts',(11.6187763833168,-1.21300082485405,0.899992820294732));
#13188=CARTESIAN_POINT('Ctrl Pts',(11.6255647330688,-1.20463460846846,0.899988745437233));
#13189=CARTESIAN_POINT('Ctrl Pts',(11.6314252437734,-1.1955686993246,0.899985180772245));
#13190=CARTESIAN_POINT('Ctrl Pts',(11.6362963259193,-1.18598144606113,0.899984461491908));
#13191=CARTESIAN_POINT('Ctrl Pts',(11.6391835002004,-1.18029891593343,0.899984035162064));
#13192=CARTESIAN_POINT('Ctrl Pts',(11.6417223485433,-1.1744324689719,0.89998453059116));
#13193=CARTESIAN_POINT('Ctrl Pts',(11.6438924319112,-1.16841525789854,0.899985826675912));
#13194=CARTESIAN_POINT('Ctrl Pts',(11.6475288754212,-1.15833212078062,0.899987998545922));
#13195=CARTESIAN_POINT('Ctrl Pts',(11.650098554646,-1.1479202064002,0.899992549671115));
#13196=CARTESIAN_POINT('Ctrl Pts',(11.6515257507029,-1.13734249630077,0.899996116295739));
#13197=CARTESIAN_POINT('Ctrl Pts',(11.6523885972688,-1.13094748084967,0.899998272586596));
#13198=CARTESIAN_POINT('Ctrl Pts',(11.6528329982118,-1.12449140232308,0.899999999966183));
#13199=CARTESIAN_POINT('Ctrl Pts',(11.6528329986453,-1.11800890309831,0.9));
#13200=CARTESIAN_POINT('Origin',(6.08275255467124,0.,0.9));
#13201=CARTESIAN_POINT('Ctrl Pts',(11.518694417043,-1.26698486563531,0.9));
#13202=CARTESIAN_POINT('Ctrl Pts',(7.83465728781595,-1.65326443611903,0.9));
#13203=CARTESIAN_POINT('Ctrl Pts',(4.1506201585889,-1.83934349355009,0.9));
#13204=CARTESIAN_POINT('Ctrl Pts',(0.466583029361856,-1.07784922788182,
0.9));
#13205=CARTESIAN_POINT('Ctrl Pts',(11.518694417043,-1.26698486563531,0.9));
#13206=CARTESIAN_POINT('Ctrl Pts',(11.516563806181,-1.26480246768431,0.941642633610146));
#13207=CARTESIAN_POINT('Ctrl Pts',(11.514433195319,-1.2626200697333,0.983285267220291));
#13208=CARTESIAN_POINT('Ctrl Pts',(11.512302584457,-1.2604376717823,1.02492790083044));
#13209=CARTESIAN_POINT('Ctrl Pts',(7.83465728781595,-1.65326443611903,0.9));
#13210=CARTESIAN_POINT('Ctrl Pts',(7.83394897884827,-1.65108203816803,0.941642633610146));
#13211=CARTESIAN_POINT('Ctrl Pts',(7.83324066988059,-1.64889964021702,0.983285267220291));
#13212=CARTESIAN_POINT('Ctrl Pts',(7.83253236091292,-1.64671724226602,1.02492790083044));
#13213=CARTESIAN_POINT('Ctrl Pts',(4.1506201585889,-1.8393434935501,0.9));
#13214=CARTESIAN_POINT('Ctrl Pts',(4.15133415151555,-1.83716109559909,0.941642633610146));
#13215=CARTESIAN_POINT('Ctrl Pts',(4.15204814444219,-1.83497869764808,0.983285267220291));
#13216=CARTESIAN_POINT('Ctrl Pts',(4.15276213736883,-1.83279629969708,1.02492790083044));
#13217=CARTESIAN_POINT('Ctrl Pts',(0.466583029361856,-1.07784922788182,
0.9));
#13218=CARTESIAN_POINT('Ctrl Pts',(0.468719324182819,-1.07566682993082,
0.941642633610146));
#13219=CARTESIAN_POINT('Ctrl Pts',(0.470855619003783,-1.07348443197981,
0.983285267220291));
#13220=CARTESIAN_POINT('Ctrl Pts',(0.472991913824746,-1.07130203402881,
1.02492790083044));
#13221=CARTESIAN_POINT('',(0.,0.,0.));
#13222=CARTESIAN_POINT('Origin',(0.,0.,0.));
#13223=CARTESIAN_POINT('',(-0.14652705620645,9.44412402177196E-5,0.0160655045842905));
#13224=CARTESIAN_POINT('',(-0.146479946776166,0.000162062070299865,0.00893449541571059));
#13225=CARTESIAN_POINT('',(-0.14635,-1.79227059055215E-17,0.));
#13226=CARTESIAN_POINT('',(0.0634007094575209,0.131904027763685,0.));
#13227=CARTESIAN_POINT('Ctrl Pts',(-0.14652705620645,9.44412402177196E-5,
0.0160655045842905));
#13228=CARTESIAN_POINT('Ctrl Pts',(-0.146560923555419,0.00502618404349199,
0.0157963945919035));
#13229=CARTESIAN_POINT('Ctrl Pts',(-0.146333578783787,0.00995455679532004,
0.0155272845995164));
#13230=CARTESIAN_POINT('Ctrl Pts',(-0.14583475180505,0.0148550342388422,
0.0152581746071293));
#13231=CARTESIAN_POINT('Ctrl Pts',(-0.140929468554047,0.0630445487404258,
0.0126118447280274));
#13232=CARTESIAN_POINT('Ctrl Pts',(-0.10977174472993,0.108536575508351,
0.0099655148489255));
#13233=CARTESIAN_POINT('Ctrl Pts',(-0.0666135938566871,0.13056551637767,
0.00731918496982359));
#13234=CARTESIAN_POINT('Ctrl Pts',(-0.0268248419338395,0.150874636338504,
0.00487945664654906));
#13235=CARTESIAN_POINT('Ctrl Pts',(0.0231637104697219,0.151241233100125,
0.00243972832327453));
#13236=CARTESIAN_POINT('Ctrl Pts',(0.0635546915223951,0.132092229195826,
-2.16840434497101E-19));
#13237=CARTESIAN_POINT('',(-0.0634007094575146,0.131904027763688,0.));
#13238=CARTESIAN_POINT('Origin',(0.,0.,0.));
#13239=CARTESIAN_POINT('Ctrl Pts',(-0.0634007094575145,0.131904027763688,
-3.88578058618805E-16));
#13240=CARTESIAN_POINT('Ctrl Pts',(-0.107282641710421,0.110811831533068,
0.00264738937425961));
#13241=CARTESIAN_POINT('Ctrl Pts',(-0.139432201149969,0.0662847592091173,
0.00529477874851962));
#13242=CARTESIAN_POINT('Ctrl Pts',(-0.145436119191498,0.0182745223106641,
0.00794216812277962));
#13243=CARTESIAN_POINT('Ctrl Pts',(-0.146186273512714,0.0122759249909008,
0.00827294388708994));
#13244=CARTESIAN_POINT('Ctrl Pts',(-0.146528267289359,0.00622295186417552,
0.00860371965140026));
#13245=CARTESIAN_POINT('Ctrl Pts',(-0.146479946776166,0.000162062070299865,
0.00893449541571059));
#13246=CARTESIAN_POINT('Origin',(0.,0.,0.));
#13247=CARTESIAN_POINT('',(-0.146148830924315,7.59978318484386E-5,0.0660655045842905));
#13248=CARTESIAN_POINT('',(-0.146133770585873,6.2751561688711E-5,0.0589344954157103));
#13249=CARTESIAN_POINT('',(-0.14635,-1.79227059055215E-17,0.));
#13250=CARTESIAN_POINT('Ctrl Pts',(-0.146148830924315,7.59978318484386E-5,
0.0660655045842905));
#13251=CARTESIAN_POINT('Ctrl Pts',(-0.146240443598182,0.0195917497831913,
0.0650077071998482));
#13252=CARTESIAN_POINT('Ctrl Pts',(-0.142607114239671,0.0390747476468127,
0.0639499098154059));
#13253=CARTESIAN_POINT('Ctrl Pts',(-0.135087779856993,0.056920264102034,
0.0628921124309636));
#13254=CARTESIAN_POINT('Ctrl Pts',(-0.116276389754784,0.10156503643559,
0.0602457825518617));
#13255=CARTESIAN_POINT('Ctrl Pts',(-0.073143724514267,0.135961331060063,
0.0575994526727599));
#13256=CARTESIAN_POINT('Ctrl Pts',(-0.025432083612881,0.144366623974243,
0.054953122793658));
#13257=CARTESIAN_POINT('Ctrl Pts',(0.0222795572885053,0.152771916888423,
0.0523067929145561));
#13258=CARTESIAN_POINT('Ctrl Pts',(0.0745701738507606,0.135186208092309,
0.0496604630354541));
#13259=CARTESIAN_POINT('Ctrl Pts',(0.107505148494886,0.0996564726649905,
0.0470141331563522));
#13260=CARTESIAN_POINT('Ctrl Pts',(0.140440123139012,0.0641267372376721,
0.0443678032772503));
#13261=CARTESIAN_POINT('Ctrl Pts',(0.154019455865009,0.010652975179149,
0.0417214733981484));
#13262=CARTESIAN_POINT('Ctrl Pts',(0.14202839331759,-0.0362847016460775,
0.0390751435190465));
#13263=CARTESIAN_POINT('Ctrl Pts',(0.130037330770172,-0.0832223784713041,
0.0364288136399446));
#13264=CARTESIAN_POINT('Ctrl Pts',(0.0924758729493388,-0.123623970063234,
0.0337824837608427));
#13265=CARTESIAN_POINT('Ctrl Pts',(0.0465351214488668,-0.139005253038876,
0.0311361538817407));
#13266=CARTESIAN_POINT('Ctrl Pts',(0.000594369948394902,-0.154386536014517,
0.0284898240026388));
#13267=CARTESIAN_POINT('Ctrl Pts',(-0.0537256752317158,-0.144747510373871,
0.025843494123537));
#13268=CARTESIAN_POINT('Ctrl Pts',(-0.0915592764828275,-0.114484496435928,
0.0231971642444351));
#13269=CARTESIAN_POINT('Ctrl Pts',(-0.125545511528741,-0.0872989822136326,
0.0208199443577202));
#13270=CARTESIAN_POINT('Ctrl Pts',(-0.146227884351973,-0.0434707826450544,
0.0184427244710054));
#13271=CARTESIAN_POINT('Ctrl Pts',(-0.14652705620645,9.44412402177196E-5,
0.0160655045842905));
#13272=CARTESIAN_POINT('Ctrl Pts',(-0.146479946776166,0.000162062070299865,
0.00893449541571059));
#13273=CARTESIAN_POINT('Ctrl Pts',(-0.146141530330399,-0.0422858476614564,
0.0112511090256603));
#13274=CARTESIAN_POINT('Ctrl Pts',(-0.126658161292025,-0.0851220706608281,
0.0135677226356099));
#13275=CARTESIAN_POINT('Ctrl Pts',(-0.0941604943243988,-0.112386678841155,
0.0158843362455596));
#13276=CARTESIAN_POINT('Ctrl Pts',(-0.0570226747722624,-0.143544241621566,
0.0185317256198196));
#13277=CARTESIAN_POINT('Ctrl Pts',(-0.00288875902448078,-0.154365965709432,
0.0211791149940796));
#13278=CARTESIAN_POINT('Ctrl Pts',(0.0434083729543798,-0.140002007265973,
0.0238265043683396));
#13279=CARTESIAN_POINT('Ctrl Pts',(0.0897055049332404,-0.125638048822514,
0.0264738937425996));
#13280=CARTESIAN_POINT('Ctrl Pts',(0.12816585314318,-0.0860884078477292,
0.0291212831168596));
#13281=CARTESIAN_POINT('Ctrl Pts',(0.141191617966992,-0.0394144013492358,
0.0317686724911196));
#13282=CARTESIAN_POINT('Ctrl Pts',(0.154217382790803,0.00725960514925768,
0.0344160618653796));
#13283=CARTESIAN_POINT('Ctrl Pts',(0.141808564228487,0.0610579771714599,
0.0370634512396396));
#13284=CARTESIAN_POINT('Ctrl Pts',(0.109639063769471,0.0973098477439542,
0.0397108406138996));
#13285=CARTESIAN_POINT('Ctrl Pts',(0.0774695633104545,0.133561718316448,
0.0423582299881596));
#13286=CARTESIAN_POINT('Ctrl Pts',(0.0255393809547383,0.152267087439235,
0.0450056193624196));
#13287=CARTESIAN_POINT('Ctrl Pts',(-0.0223595433272462,0.144872892294413,
0.0476530087366796));
#13288=CARTESIAN_POINT('Ctrl Pts',(-0.070258467609231,0.137478697149591,
0.0503003981109396));
#13289=CARTESIAN_POINT('Ctrl Pts',(-0.114126133817484,0.10398493773716,
0.0529477874851996));
#13290=CARTESIAN_POINT('Ctrl Pts',(-0.133871661545403,0.059725601630819,
0.0555951768594596));
#13291=CARTESIAN_POINT('Ctrl Pts',(-0.142173753131161,0.0411165744656389,
0.0567082830448765));
#13292=CARTESIAN_POINT('Ctrl Pts',(-0.146211489678532,0.0206043892842972,
0.0578213892302934));
#13293=CARTESIAN_POINT('Ctrl Pts',(-0.146133770585873,6.2751561688711E-5,
0.0589344954157103));
#13294=CARTESIAN_POINT('Origin',(0.,0.,0.));
#13295=CARTESIAN_POINT('',(-0.146252097264499,-0.000124487410312429,0.116065504584291));
#13296=CARTESIAN_POINT('',(-0.146276374479508,-0.000129480650117819,0.10893449541571));
#13297=CARTESIAN_POINT('',(-0.14635,-1.79227059055215E-17,0.));
#13298=CARTESIAN_POINT('Ctrl Pts',(-0.146252097264499,-0.000124487410312429,
0.116065504584291));
#13299=CARTESIAN_POINT('Ctrl Pts',(-0.145977101830714,0.0338815411246725,
0.114219019807793));
#13300=CARTESIAN_POINT('Ctrl Pts',(-0.134160879762789,0.0680598926014691,
0.112372535031295));
#13301=CARTESIAN_POINT('Ctrl Pts',(-0.112484833627769,0.0939988017516943,
0.110526050254798));
#13302=CARTESIAN_POINT('Ctrl Pts',(-0.0814193359437304,0.131173714423195,
0.107879720375696));
#13303=CARTESIAN_POINT('Ctrl Pts',(-0.0301019434218634,0.151424966146533,
0.105233390496594));
#13304=CARTESIAN_POINT('Ctrl Pts',(0.0179785702873004,0.145483266051774,
0.102587060617492));
#13305=CARTESIAN_POINT('Ctrl Pts',(0.0660590839964643,0.139541565957016,
0.0999407307383904));
#13306=CARTESIAN_POINT('Ctrl Pts',(0.110902718892925,0.107406914044162,
0.0972944008592884));
#13307=CARTESIAN_POINT('Ctrl Pts',(0.131983829661647,0.0637877973597534,
0.0946480709801865));
#13308=CARTESIAN_POINT('Ctrl Pts',(0.15306494043037,0.0201686806753445,
0.0920017411010846));
#13309=CARTESIAN_POINT('Ctrl Pts',(0.150383527071356,-0.0349349007806195,
0.0893554112219828));
#13310=CARTESIAN_POINT('Ctrl Pts',(0.125166930059577,-0.0763010783846813,
0.0867090813428809));
#13311=CARTESIAN_POINT('Ctrl Pts',(0.0999503330477985,-0.117667255988743,
0.084062751463779));
#13312=CARTESIAN_POINT('Ctrl Pts',(0.0521985523832557,-0.145296029740903,
0.081416421584677));
#13313=CARTESIAN_POINT('Ctrl Pts',(0.00376830011669856,-0.146541450754272,
0.0787700917055751));
#13314=CARTESIAN_POINT('Ctrl Pts',(-0.0446619521498586,-0.147786871767642,
0.0761237618264732));
#13315=CARTESIAN_POINT('Ctrl Pts',(-0.09377067601843,-0.122648940042221,
0.0734774319473713));
#13316=CARTESIAN_POINT('Ctrl Pts',(-0.121079980470766,-0.0826333491581908,
0.0708311020682694));
#13317=CARTESIAN_POINT('Ctrl Pts',(-0.137473143648068,-0.0586128871159229,
0.0692425695736098));
#13318=CARTESIAN_POINT('Ctrl Pts',(-0.146011252866834,-0.02923151094855,
0.0676540370789502));
#13319=CARTESIAN_POINT('Ctrl Pts',(-0.146148830924315,7.59978318484386E-5,
0.0660655045842905));
#13320=CARTESIAN_POINT('Ctrl Pts',(-0.146133770585873,6.2751561688711E-5,
0.0589344954157103));
#13321=CARTESIAN_POINT('Ctrl Pts',(-0.146026644150963,-0.0282514289199324,
0.0604687786045534));
#13322=CARTESIAN_POINT('Ctrl Pts',(-0.138100435392092,-0.0566215672018456,
0.0620030617933965));
#13323=CARTESIAN_POINT('Ctrl Pts',(-0.122745086057252,-0.0801407530065182,
0.0635373449822396));
#13324=CARTESIAN_POINT('Ctrl Pts',(-0.0962495935935968,-0.120722858737265,
0.0661847343564996));
#13325=CARTESIAN_POINT('Ctrl Pts',(-0.0476352194187008,-0.146862157398507,
0.0688321237307596));
#13326=CARTESIAN_POINT('Ctrl Pts',(0.00082938917649622,-0.146587691816784,
0.0714795131050196));
#13327=CARTESIAN_POINT('Ctrl Pts',(0.0492939977716932,-0.146313226235061,
0.0741269024792796));
#13328=CARTESIAN_POINT('Ctrl Pts',(0.0976088407871913,-0.119624996410372,
0.0767742918535397));
#13329=CARTESIAN_POINT('Ctrl Pts',(0.123643642180798,-0.0787464320231966,
0.0794216812277997));
#13330=CARTESIAN_POINT('Ctrl Pts',(0.149678443574405,-0.0378678676360213,
0.0820690706020596));
#13331=CARTESIAN_POINT('Ctrl Pts',(0.153433203346121,0.0172010313136401,
0.0847164599763195));
#13332=CARTESIAN_POINT('Ctrl Pts',(0.133187835944515,0.06123527443138,0.0873638493505795));
#13333=CARTESIAN_POINT('Ctrl Pts',(0.11294246854291,0.10526951754912,0.0900112387248395));
#13334=CARTESIAN_POINT('Ctrl Pts',(0.0686969739679828,0.138269104834938,
0.0926586280990997));
#13335=CARTESIAN_POINT('Ctrl Pts',(0.0207181735233275,0.145118849380084,
0.0953060174733597));
#13336=CARTESIAN_POINT('Ctrl Pts',(-0.027260626921328,0.151968593925229,
0.0979534068476197));
#13337=CARTESIAN_POINT('Ctrl Pts',(-0.0789727332357116,0.132668495729702,
0.10060079622188));
#13338=CARTESIAN_POINT('Ctrl Pts',(-0.110731403441959,0.0960588230543748,
0.10324818559614));
#13339=CARTESIAN_POINT('Ctrl Pts',(-0.133469481440122,0.0698475998711364,
0.105143622202663));
#13340=CARTESIAN_POINT('Ctrl Pts',(-0.145979327216774,0.0347634013028336,
0.107039058809187));
#13341=CARTESIAN_POINT('Ctrl Pts',(-0.146276374479508,-0.000129480650117819,
0.10893449541571));
#13342=CARTESIAN_POINT('Origin',(0.,0.,0.));
#13343=CARTESIAN_POINT('',(-0.146589818999335,-3.81787486967988E-6,0.166065504584291));
#13344=CARTESIAN_POINT('',(-0.146589453522336,1.04004190909306E-5,0.15893449541571));
#13345=CARTESIAN_POINT('',(-0.14635,-1.79227059055215E-17,0.));
#13346=CARTESIAN_POINT('Ctrl Pts',(-0.146589818999335,-3.81787486967988E-6,
0.166065504584291));
#13347=CARTESIAN_POINT('Ctrl Pts',(-0.146571339149733,0.0482382848470949,
0.163430332415738));
#13348=CARTESIAN_POINT('Ctrl Pts',(-0.120433071521034,0.0964975486977609,
0.160795160247185));
#13349=CARTESIAN_POINT('Ctrl Pts',(-0.0800107885095625,0.122828684230981,
0.158159988078632));
#13350=CARTESIAN_POINT('Ctrl Pts',(-0.0394173515450545,0.149271309704865,
0.15551365819953));
#13351=CARTESIAN_POINT('Ctrl Pts',(0.0155813181737399,0.153599719825856,
0.152867328320428));
#13352=CARTESIAN_POINT('Ctrl Pts',(0.0598114643267532,0.133832733731537,
0.150220998441327));
#13353=CARTESIAN_POINT('Ctrl Pts',(0.104041610479766,0.114065747637217,
0.147574668562225));
#13354=CARTESIAN_POINT('Ctrl Pts',(0.137503233066998,0.0702033653275883,
0.144928338683123));
#13355=CARTESIAN_POINT('Ctrl Pts',(0.144880420813362,0.0223220882221681,
0.142282008804021));
#13356=CARTESIAN_POINT('Ctrl Pts',(0.152257608559726,-0.0255591888832524,
0.139635678924919));
#13357=CARTESIAN_POINT('Ctrl Pts',(0.133550361465222,-0.077459360784464,
0.136989349045817));
#13358=CARTESIAN_POINT('Ctrl Pts',(0.0973212811704284,-0.109622900294719,
0.134343019166715));
#13359=CARTESIAN_POINT('Ctrl Pts',(0.0610922008756344,-0.141786439804975,
0.131696689287613));
#13360=CARTESIAN_POINT('Ctrl Pts',(0.00734128738055008,-0.154213346924274,
0.129050359408511));
#13361=CARTESIAN_POINT('Ctrl Pts',(-0.0393288211819405,-0.141215634503184,
0.126404029529409));
#13362=CARTESIAN_POINT('Ctrl Pts',(-0.0859989297444312,-0.128217922082094,
0.123757699650308));
#13363=CARTESIAN_POINT('Ctrl Pts',(-0.125588233374328,-0.0897955901206149,
0.121111369771206));
#13364=CARTESIAN_POINT('Ctrl Pts',(-0.139976083766172,-0.043535137330043,
0.118465039892104));
#13365=CARTESIAN_POINT('Ctrl Pts',(-0.144324767489921,-0.0295530571287048,
0.117665194789499));
#13366=CARTESIAN_POINT('Ctrl Pts',(-0.146371217526823,-0.0148549394177889,
0.116865349686895));
#13367=CARTESIAN_POINT('Ctrl Pts',(-0.146252097264499,-0.000124487410312429,
0.116065504584291));
#13368=CARTESIAN_POINT('Ctrl Pts',(-0.146276374479508,-0.000129480650117819,
0.10893449541571));
#13369=CARTESIAN_POINT('Ctrl Pts',(-0.14639421831063,-0.0139720956278579,
0.109686448183447));
#13370=CARTESIAN_POINT('Ctrl Pts',(-0.14458995413065,-0.0277846002915201,
0.110438400951183));
#13371=CARTESIAN_POINT('Ctrl Pts',(-0.140739671041232,-0.041001045008257,
0.11119035371892));
#13372=CARTESIAN_POINT('Ctrl Pts',(-0.127184034336146,-0.0875319932404337,
0.11383774309318));
#13373=CARTESIAN_POINT('Ctrl Pts',(-0.0882675268278623,-0.12667464254966,
0.11648513246744));
#13374=CARTESIAN_POINT('Ctrl Pts',(-0.0418159243469935,-0.140499695546946,
0.1191325218417));
#13375=CARTESIAN_POINT('Ctrl Pts',(0.00463567813387508,-0.154324748544231,
0.12177991121596));
#13376=CARTESIAN_POINT('Ctrl Pts',(0.0586223755873289,-0.142832205229577,
0.12442730059022));
#13377=CARTESIAN_POINT('Ctrl Pts',(0.0954154960694136,-0.111286216216264,
0.12707468996448));
#13378=CARTESIAN_POINT('Ctrl Pts',(0.132208616551499,-0.0797402272029501,
0.12972207933874));
#13379=CARTESIAN_POINT('Ctrl Pts',(0.151808160062214,-0.0281407924909768,
0.132369468712999));
#13380=CARTESIAN_POINT('Ctrl Pts',(0.145236524363737,0.0198768833792122,
0.135016858087259));
#13381=CARTESIAN_POINT('Ctrl Pts',(0.138664888665259,0.0678945592494009,
0.13766424746152));
#13382=CARTESIAN_POINT('Ctrl Pts',(0.105922073757589,0.112330476277805,
0.14031163683578));
#13383=CARTESIAN_POINT('Ctrl Pts',(0.062005973158836,0.132830708741579,
0.14295902621004));
#13384=CARTESIAN_POINT('Ctrl Pts',(0.0180898725600832,0.153330941205352,
0.1456064155843));
#13385=CARTESIAN_POINT('Ctrl Pts',(-0.0369995137297515,0.149895489104495,
0.14825380495856));
#13386=CARTESIAN_POINT('Ctrl Pts',(-0.0780284182758478,0.124097962381086,
0.15090119433282));
#13387=CARTESIAN_POINT('Ctrl Pts',(-0.119057322821944,0.0983004356576776,
0.153548583707079));
#13388=CARTESIAN_POINT('Ctrl Pts',(-0.146025745624302,0.0501408343117172,
0.15619597308134));
#13389=CARTESIAN_POINT('Ctrl Pts',(-0.14658076309025,0.00167873146180186,
0.1588433624556));
#13390=CARTESIAN_POINT('Ctrl Pts',(-0.146587131676737,0.00112264969450139,
0.15887374010897));
#13391=CARTESIAN_POINT('Ctrl Pts',(-0.146590022522527,0.000566528098114988,
0.15890411776234));
#13392=CARTESIAN_POINT('Ctrl Pts',(-0.146589453522336,1.04004190909306E-5,
0.15893449541571));
#13393=CARTESIAN_POINT('Origin',(0.,0.,0.));
#13394=CARTESIAN_POINT('',(-0.146263250741535,0.000126870157254357,0.21606550458429));
#13395=CARTESIAN_POINT('',(-0.146245769975643,0.000123264779366826,0.20893449541571));
#13396=CARTESIAN_POINT('',(-0.14635,-1.79227059055215E-17,0.));
#13397=CARTESIAN_POINT('Ctrl Pts',(-0.146263250741535,0.000126870157254357,
0.21606550458429));
#13398=CARTESIAN_POINT('Ctrl Pts',(-0.146381923100139,0.0144435832128767,
0.215287974902784));
#13399=CARTESIAN_POINT('Ctrl Pts',(-0.144450237714319,0.0287289633064517,
0.214510445221278));
#13400=CARTESIAN_POINT('Ctrl Pts',(-0.140337374518256,0.0423560295890773,
0.213732915539772));
#13401=CARTESIAN_POINT('Ctrl Pts',(-0.126339204386259,0.0887358830222778,
0.21108658566067));
#13402=CARTESIAN_POINT('Ctrl Pts',(-0.0870745347363382,0.127489909020004,
0.208440255781569));
#13403=CARTESIAN_POINT('Ctrl Pts',(-0.0405154226099946,0.140879780169064,
0.205793925902467));
#13404=CARTESIAN_POINT('Ctrl Pts',(0.00604368951634975,0.154269651318124,
0.203147596023365));
#13405=CARTESIAN_POINT('Ctrl Pts',(0.0598972441191175,0.142295367618517,
0.200501266144263));
#13406=CARTESIAN_POINT('Ctrl Pts',(0.0963956219934077,0.110437747119808,
0.197854936265161));
#13407=CARTESIAN_POINT('Ctrl Pts',(0.132893999867697,0.0785801266211,0.195208606386059));
#13408=CARTESIAN_POINT('Ctrl Pts',(0.15203720101351,0.0268391693232909,
0.192562276506957));
#13409=CARTESIAN_POINT('Ctrl Pts',(0.145063081087281,-0.0211024746124516,
0.189915946627855));
#13410=CARTESIAN_POINT('Ctrl Pts',(0.138088961161051,-0.0690441185481943,
0.187269616748753));
#13411=CARTESIAN_POINT('Ctrl Pts',(0.10499752016278,-0.11318644912187,0.184623286869651));
#13412=CARTESIAN_POINT('Ctrl Pts',(0.060935231264163,-0.133324827106958,
0.181976956990549));
#13413=CARTESIAN_POINT('Ctrl Pts',(0.0168729423655461,-0.153463205092045,
0.179330627111448));
#13414=CARTESIAN_POINT('Ctrl Pts',(-0.0381601944334158,-0.149597630488544,
0.176684297232346));
#13415=CARTESIAN_POINT('Ctrl Pts',(-0.0789746466099193,-0.123497437688695,
0.174037967353244));
#13416=CARTESIAN_POINT('Ctrl Pts',(-0.119961184605052,-0.0972871987457574,
0.171380479763593));
#13417=CARTESIAN_POINT('Ctrl Pts',(-0.146608455341797,-0.0486544490602708,
0.168722992173942));
#13418=CARTESIAN_POINT('Ctrl Pts',(-0.146589818999335,-3.81787486967988E-6,
0.166065504584291));
#13419=CARTESIAN_POINT('Ctrl Pts',(-0.146589453522336,1.04004190909306E-5,
0.15893449541571));
#13420=CARTESIAN_POINT('Ctrl Pts',(-0.146540434588914,-0.0478995759235739,
0.1615515071366));
#13421=CARTESIAN_POINT('Ctrl Pts',(-0.120813506558866,-0.0958546957256878,
0.16416851885749));
#13422=CARTESIAN_POINT('Ctrl Pts',(-0.0808500697395765,-0.122278388912248,
0.16678553057838));
#13423=CARTESIAN_POINT('Ctrl Pts',(-0.0404227467934142,-0.149008802082514,
0.16943291995264));
#13424=CARTESIAN_POINT('Ctrl Pts',(0.0145735112284506,-0.153705024069172,
0.1720803093269));
#13425=CARTESIAN_POINT('Ctrl Pts',(0.0589475933459444,-0.134215943447351,
0.17472769870116));
#13426=CARTESIAN_POINT('Ctrl Pts',(0.103321675463438,-0.11472686282553,
0.17737508807542));
#13427=CARTESIAN_POINT('Ctrl Pts',(0.137073581676561,-0.0710524795952304,
0.18002247744968));
#13428=CARTESIAN_POINT('Ctrl Pts',(0.144743205110219,-0.0231979049720499,
0.18266986682394));
#13429=CARTESIAN_POINT('Ctrl Pts',(0.152412828543877,0.024656669651131,
0.1853172561982));
#13430=CARTESIAN_POINT('Ctrl Pts',(0.13400016919807,0.0766914356671922,
0.18796464557246));
#13431=CARTESIAN_POINT('Ctrl Pts',(0.0979391709064228,0.109071797518936,
0.19061203494672));
#13432=CARTESIAN_POINT('Ctrl Pts',(0.0618781726147763,0.141452159370678,
0.19325942432098));
#13433=CARTESIAN_POINT('Ctrl Pts',(0.00816883537729064,0.154178117058104,
0.195906813695239));
#13434=CARTESIAN_POINT('Ctrl Pts',(-0.0385872054932313,0.1414205281901,
0.198554203069499));
#13435=CARTESIAN_POINT('Ctrl Pts',(-0.0853432463637543,0.128662939322095,
0.201201592443759));
#13436=CARTESIAN_POINT('Ctrl Pts',(-0.125145990867313,0.0904218038986596,
0.20384898181802));
#13437=CARTESIAN_POINT('Ctrl Pts',(-0.139763737461459,0.0442135263146365,
0.20649637119228));
#13438=CARTESIAN_POINT('Ctrl Pts',(-0.144251162244238,0.030028291356252,
0.207309079266757));
#13439=CARTESIAN_POINT('Ctrl Pts',(-0.146365162502875,0.0150922359825044,
0.208121787341234));
#13440=CARTESIAN_POINT('Ctrl Pts',(-0.146245769975643,0.000123264779366826,
0.20893449541571));
#13441=CARTESIAN_POINT('Origin',(0.,0.,0.));
#13442=CARTESIAN_POINT('',(-0.146142672279203,-7.01165389862951E-5,0.266065504584291));
#13443=CARTESIAN_POINT('',(-0.146150215784492,-7.74481165901552E-5,0.258934495415711));
#13444=CARTESIAN_POINT('',(-0.14635,-1.79227059055215E-17,0.));
#13445=CARTESIAN_POINT('Ctrl Pts',(-0.146142672279203,-7.01165389862951E-5,
0.266065504584291));
#13446=CARTESIAN_POINT('Ctrl Pts',(-0.146017527260215,0.028828671850369,
0.264499287510729));
#13447=CARTESIAN_POINT('Ctrl Pts',(-0.137733916992107,0.0577936173630845,
0.262933070437168));
#13448=CARTESIAN_POINT('Ctrl Pts',(-0.121770841384076,0.0816117278206753,
0.261366853363607));
#13449=CARTESIAN_POINT('Ctrl Pts',(-0.0947991242083451,0.121855560193383,
0.258720523484505));
#13450=CARTESIAN_POINT('Ctrl Pts',(-0.0459036471244643,0.147405924851771,
0.256074193605403));
#13451=CARTESIAN_POINT('Ctrl Pts',(0.0025353607453442,0.146568017913755,
0.253427863726301));
#13452=CARTESIAN_POINT('Ctrl Pts',(0.050974368615152,0.145730110975738,
0.250781533847199));
#13453=CARTESIAN_POINT('Ctrl Pts',(0.0989569072708876,0.118503932441319,
0.248135203968097));
#13454=CARTESIAN_POINT('Ctrl Pts',(0.124520613871998,0.0773513325689396,
0.245488874088995));
#13455=CARTESIAN_POINT('Ctrl Pts',(0.150084320473109,0.0361987326965595,
0.242842544209893));
#13456=CARTESIAN_POINT('Ctrl Pts',(0.153229195019594,-0.0188802885137813,
0.240196214330791));
#13457=CARTESIAN_POINT('Ctrl Pts',(0.132515778953886,-0.0626751965094481,
0.237549884451689));
#13458=CARTESIAN_POINT('Ctrl Pts',(0.111802362888177,-0.106470104505115,
0.234903554572587));
#13459=CARTESIAN_POINT('Ctrl Pts',(0.0672306562102751,-0.138980899286108,
0.232257224693486));
#13460=CARTESIAN_POINT('Ctrl Pts',(0.0192018303028616,-0.145326878595667,
0.229610894814384));
#13461=CARTESIAN_POINT('Ctrl Pts',(-0.0288269956045516,-0.151672857905225,
0.226964564935282));
#13462=CARTESIAN_POINT('Ctrl Pts',(-0.0803129407414762,-0.131854021743351,
0.22431823505618));
#13463=CARTESIAN_POINT('Ctrl Pts',(-0.111690078002902,-0.0949417632280756,
0.221671905177078));
#13464=CARTESIAN_POINT('Ctrl Pts',(-0.133848162215005,-0.0688748557907962,
0.219803104979482));
#13465=CARTESIAN_POINT('Ctrl Pts',(-0.145978020566425,-0.0342834897603843,
0.217934304781886));
#13466=CARTESIAN_POINT('Ctrl Pts',(-0.146263250741535,0.000126870157254357,
0.21606550458429));
#13467=CARTESIAN_POINT('Ctrl Pts',(-0.146245769975643,0.000123264779366826,
0.20893449541571));
#13468=CARTESIAN_POINT('Ctrl Pts',(-0.145976242399967,-0.03366905549635,
0.210769176715493));
#13469=CARTESIAN_POINT('Ctrl Pts',(-0.134324750276972,-0.067629123606452,
0.212603858015276));
#13470=CARTESIAN_POINT('Ctrl Pts',(-0.112902327433,-0.0934976078712483,
0.214438539315059));
#13471=CARTESIAN_POINT('Ctrl Pts',(-0.0819904221256615,-0.130825044728502,
0.217085928689319));
#13472=CARTESIAN_POINT('Ctrl Pts',(-0.0307338628262512,-0.151304498698398,
0.21973331806358));
#13473=CARTESIAN_POINT('Ctrl Pts',(0.0173892134168267,-0.145555327884408,
0.22238070743784));
#13474=CARTESIAN_POINT('Ctrl Pts',(0.0655122896599044,-0.139806157070418,
0.2250280968121));
#13475=CARTESIAN_POINT('Ctrl Pts',(0.11050188284665,-0.107828361472542,
0.22767548618636));
#13476=CARTESIAN_POINT('Ctrl Pts',(0.131750448317205,-0.0642694140823833,
0.23032287556062));
#13477=CARTESIAN_POINT('Ctrl Pts',(0.15299901378776,-0.020710466692225,
0.232970264934879));
#13478=CARTESIAN_POINT('Ctrl Pts',(0.150506551542124,0.0344296324902152,
0.23561765430914));
#13479=CARTESIAN_POINT('Ctrl Pts',(0.125414737320077,0.0758938856636754,
0.2382650436834));
#13480=CARTESIAN_POINT('Ctrl Pts',(0.10032292309803,0.117358138837136,0.24091243305766));
#13481=CARTESIAN_POINT('Ctrl Pts',(0.0526317568995709,0.145146546001616,
0.24355982243192));
#13482=CARTESIAN_POINT('Ctrl Pts',(0.00418624259284972,0.146530589268381,
0.24620721180618));
#13483=CARTESIAN_POINT('Ctrl Pts',(-0.0442592717138715,0.147914632535146,
0.24885460118044));
#13484=CARTESIAN_POINT('Ctrl Pts',(-0.0934591341288551,0.122894311904195,
0.2515019905547));
#13485=CARTESIAN_POINT('Ctrl Pts',(-0.120877280418781,0.082930219442967,
0.25414937992896));
#13486=CARTESIAN_POINT('Ctrl Pts',(-0.137396572682769,0.0588520590724165,
0.255744418424543));
#13487=CARTESIAN_POINT('Ctrl Pts',(-0.146009100715185,0.0293493086505574,
0.257339456920127));
#13488=CARTESIAN_POINT('Ctrl Pts',(-0.146150215784492,-7.74481165901552E-5,
0.258934495415711));
#13489=CARTESIAN_POINT('Origin',(0.,0.,0.));
#13490=CARTESIAN_POINT('',(-0.146519404976022,-8.97763884284003E-5,0.316065504584291));
#13491=CARTESIAN_POINT('',(-0.146528765763263,-8.45393868379275E-5,0.30893449541571));
#13492=CARTESIAN_POINT('',(-0.14635,-1.79227059055215E-17,0.));
#13493=CARTESIAN_POINT('Ctrl Pts',(-0.146519404976022,-8.97763884284003E-5,
0.316065504584291));
#13494=CARTESIAN_POINT('Ctrl Pts',(-0.146208092107557,0.043076445171776,
0.313710600118674));
#13495=CARTESIAN_POINT('Ctrl Pts',(-0.125958424314353,0.0864965766126209,
0.311355695653057));
#13496=CARTESIAN_POINT('Ctrl Pts',(-0.0925183485457987,0.1137056160074,
0.309000791187441));
#13497=CARTESIAN_POINT('Ctrl Pts',(-0.0549399784004991,0.144281843189175,
0.306354461308339));
#13498=CARTESIAN_POINT('Ctrl Pts',(-0.00070450021881692,0.154386382754941,
0.303708131429237));
#13499=CARTESIAN_POINT('Ctrl Pts',(0.0453636543616171,0.139394227973128,
0.301061801550135));
#13500=CARTESIAN_POINT('Ctrl Pts',(0.0914318089420511,0.124402073191315,
0.298415471671033));
#13501=CARTESIAN_POINT('Ctrl Pts',(0.129332639921237,0.0843132240619223,
0.295769141791931));
#13502=CARTESIAN_POINT('Ctrl Pts',(0.141718340675246,0.0374769775398043,
0.293122811912829));
#13503=CARTESIAN_POINT('Ctrl Pts',(0.154104041429255,-0.00935926898231351,
0.290476482033727));
#13504=CARTESIAN_POINT('Ctrl Pts',(0.140974611958088,-0.0629429128971569,
0.287830152154626));
#13505=CARTESIAN_POINT('Ctrl Pts',(0.108339598692885,-0.0987478773661917,
0.285183822275524));
#13506=CARTESIAN_POINT('Ctrl Pts',(0.0757045854276824,-0.134552841835227,
0.282537492396422));
#13507=CARTESIAN_POINT('Ctrl Pts',(0.0235639883684441,-0.152579126858453,
0.27989116251732));
#13508=CARTESIAN_POINT('Ctrl Pts',(-0.0242166208952047,-0.144575818177467,
0.277244832638218));
#13509=CARTESIAN_POINT('Ctrl Pts',(-0.0719972301588528,-0.136572509496481,
0.274598502759116));
#13510=CARTESIAN_POINT('Ctrl Pts',(-0.115417851626912,-0.102539607111283,
0.271952172880014));
#13511=CARTESIAN_POINT('Ctrl Pts',(-0.13460418372715,-0.0580545058751705,
0.269305843000912));
#13512=CARTESIAN_POINT('Ctrl Pts',(-0.142435181350113,-0.0398976888130428,
0.268225730195372));
#13513=CARTESIAN_POINT('Ctrl Pts',(-0.146228976240411,-0.0199996345674016,
0.267145617389831));
#13514=CARTESIAN_POINT('Ctrl Pts',(-0.146142672279203,-7.01165389862951E-5,
0.266065504584291));
#13515=CARTESIAN_POINT('Ctrl Pts',(-0.146150215784492,-7.74481165901552E-5,
0.258934495415711));
#13516=CARTESIAN_POINT('Ctrl Pts',(-0.146243318595233,-0.0194921979337541,
0.259986846294387));
#13517=CARTESIAN_POINT('Ctrl Pts',(-0.142648899141753,-0.0388738684647463,
0.261039197173063));
#13518=CARTESIAN_POINT('Ctrl Pts',(-0.135204796371803,-0.0566427511368837,
0.26209154805174));
#13519=CARTESIAN_POINT('Ctrl Pts',(-0.116477735870028,-0.101343764964001,
0.264738937426));
#13520=CARTESIAN_POINT('Ctrl Pts',(-0.0733871847016099,-0.135837928326728,
0.26738632680026));
#13521=CARTESIAN_POINT('Ctrl Pts',(-0.0256708287318585,-0.144325142544676,
0.27003371617452));
#13522=CARTESIAN_POINT('Ctrl Pts',(0.0220455272378925,-0.152812356762624,
0.27268110554878));
#13523=CARTESIAN_POINT('Ctrl Pts',(0.0743876880089763,-0.135292621835792,
0.27532849492304));
#13524=CARTESIAN_POINT('Ctrl Pts',(0.10738025529095,-0.0997908762961729,
0.2779758842973));
#13525=CARTESIAN_POINT('Ctrl Pts',(0.140372822572925,-0.0642891307565533,
0.280623273671559));
#13526=CARTESIAN_POINT('Ctrl Pts',(0.154015796365789,-0.010805374604146,
0.283270663045819));
#13527=CARTESIAN_POINT('Ctrl Pts',(0.142059993874458,0.0361620845457957,
0.285918052420079));
#13528=CARTESIAN_POINT('Ctrl Pts',(0.130104191383128,0.0831295436957373,
0.288565441794339));
#13529=CARTESIAN_POINT('Ctrl Pts',(0.0925496126076039,0.123580705843213,
0.291212831168599));
#13530=CARTESIAN_POINT('Ctrl Pts',(0.0465981836912963,0.138986860871753,
0.29386022054286));
#13531=CARTESIAN_POINT('Ctrl Pts',(0.000646754774988913,0.154393015900293,
0.296507609917119));
#13532=CARTESIAN_POINT('Ctrl Pts',(-0.0537015242821025,0.144754163809898,
0.29915499929138));
#13533=CARTESIAN_POINT('Ctrl Pts',(-0.0915523499663989,0.114485393976436,
0.30180238866564));
#13534=CARTESIAN_POINT('Ctrl Pts',(-0.125542580994678,0.0873038870745135,
0.30417975758233));
#13535=CARTESIAN_POINT('Ctrl Pts',(-0.146229051243382,0.0434861464246214,
0.30655712649902));
#13536=CARTESIAN_POINT('Ctrl Pts',(-0.146528765763263,-8.45393868379275E-5,
0.30893449541571));
#13537=CARTESIAN_POINT('Origin',(0.,0.,0.));
#13538=CARTESIAN_POINT('',(-0.146416087288192,0.000126442170093593,0.366065504584291));
#13539=CARTESIAN_POINT('',(-0.146408012399712,0.000128195943346294,0.358934495415711));
#13540=CARTESIAN_POINT('',(-0.14635,-1.79227059055215E-17,0.));
#13541=CARTESIAN_POINT('Ctrl Pts',(-0.146416087288192,0.000126442170093593,
0.366065504584291));
#13542=CARTESIAN_POINT('Ctrl Pts',(-0.146499294961499,0.00925816812376314,
0.365568242605721));
#13543=CARTESIAN_POINT('Ctrl Pts',(-0.145718277739785,0.0183757049974218,
0.365070980627151));
#13544=CARTESIAN_POINT('Ctrl Pts',(-0.144021710151773,0.0273195705351122,
0.364573718648581));
#13545=CARTESIAN_POINT('Ctrl Pts',(-0.134992913071845,0.0749170536065741,
0.361927388769479));
#13546=CARTESIAN_POINT('Ctrl Pts',(-0.100034284522917,0.117595890322328,
0.359281058890377));
#13547=CARTESIAN_POINT('Ctrl Pts',(-0.0551469387876206,0.135821305661589,
0.356634729011275));
#13548=CARTESIAN_POINT('Ctrl Pts',(-0.0102595930523245,0.15404672100085,
0.353988399132173));
#13549=CARTESIAN_POINT('Ctrl Pts',(0.0445564698693406,0.147818714963618,
0.351342069253072));
#13550=CARTESIAN_POINT('Ctrl Pts',(0.0842110755700531,0.119987943896873,
0.34869573937397));
#13551=CARTESIAN_POINT('Ctrl Pts',(0.123865681270766,0.0921571728301272,
0.346049409494868));
#13552=CARTESIAN_POINT('Ctrl Pts',(0.148358829750526,0.0427236367338667,
0.343403079615766));
#13553=CARTESIAN_POINT('Ctrl Pts',(0.146479621605269,-0.00568615719458776,
0.340756749736664));
#13554=CARTESIAN_POINT('Ctrl Pts',(0.144600413460012,-0.0540959511230416,
0.338110419857562));
#13555=CARTESIAN_POINT('Ctrl Pts',(0.116348848689739,-0.101482002883689,
0.33546408997846));
#13556=CARTESIAN_POINT('Ctrl Pts',(0.0746561129649502,-0.126154971072205,
0.332817760099358));
#13557=CARTESIAN_POINT('Ctrl Pts',(0.0329633772401616,-0.150827939260721,
0.330171430220256));
#13558=CARTESIAN_POINT('Ctrl Pts',(-0.0221705294391424,-0.152787823877104,
0.327525100341154));
#13559=CARTESIAN_POINT('Ctrl Pts',(-0.0655099505772086,-0.131137554898038,
0.324878770462052));
#13560=CARTESIAN_POINT('Ctrl Pts',(-0.108849371715275,-0.109487285918972,
0.322232440582951));
#13561=CARTESIAN_POINT('Ctrl Pts',(-0.140394307312104,-0.0642268633444555,
0.319586110703849));
#13562=CARTESIAN_POINT('Ctrl Pts',(-0.14570614405606,-0.0160726946583056,
0.316939780824747));
#13563=CARTESIAN_POINT('Ctrl Pts',(-0.146291106736525,-0.0107697471190636,
0.316648355411261));
#13564=CARTESIAN_POINT('Ctrl Pts',(-0.146557930734812,-0.0054317060295066,
0.316356929997776));
#13565=CARTESIAN_POINT('Ctrl Pts',(-0.146519404976022,-8.97763884284003E-5,
0.316065504584291));
#13566=CARTESIAN_POINT('Ctrl Pts',(-0.146528765763263,-8.45393868379275E-5,
0.30893449541571));
#13567=CARTESIAN_POINT('Ctrl Pts',(-0.146562807199252,-0.00503327764821679,
0.30920451587328));
#13568=CARTESIAN_POINT('Ctrl Pts',(-0.14633385314783,-0.00997882882536714,
0.30947453633085));
#13569=CARTESIAN_POINT('Ctrl Pts',(-0.145831525524598,-0.0148964553326841,
0.309744556788419));
#13570=CARTESIAN_POINT('Ctrl Pts',(-0.140906503086998,-0.0631108472318147,
0.312391946162679));
#13571=CARTESIAN_POINT('Ctrl Pts',(-0.109703085900295,-0.108640943453547,
0.31503933553694));
#13572=CARTESIAN_POINT('Ctrl Pts',(-0.0665140418604196,-0.13063162118607,
0.3176867249112));
#13573=CARTESIAN_POINT('Ctrl Pts',(-0.0233249978205455,-0.152622298918592,
0.32033411428546));
#13574=CARTESIAN_POINT('Ctrl Pts',(0.0318496730725009,-0.151073558161906,
0.322981503659719));
#13575=CARTESIAN_POINT('Ctrl Pts',(0.0737371373950496,-0.126694801736668,
0.325628893033979));
#13576=CARTESIAN_POINT('Ctrl Pts',(0.115624601717599,-0.10231604531143,
0.328276282408239));
#13577=CARTESIAN_POINT('Ctrl Pts',(0.144224859469651,-0.0551072732176397,
0.3309236717825));
#13578=CARTESIAN_POINT('Ctrl Pts',(0.146437523492708,-0.0066925280449658,
0.33357106115676));
#13579=CARTESIAN_POINT('Ctrl Pts',(0.148650187515766,0.0417222171277085,
0.33621845053102));
#13580=CARTESIAN_POINT('Ctrl Pts',(0.124475257809829,0.0913429353792657,
0.33886583990528));
#13581=CARTESIAN_POINT('Ctrl Pts',(0.0849860939726622,0.119440788885456,
0.34151322927954));
#13582=CARTESIAN_POINT('Ctrl Pts',(0.0454969301354961,0.147538642391646,
0.344160618653799));
#13583=CARTESIAN_POINT('Ctrl Pts',(-0.00930646783289898,0.154113631152469,
0.346808008028059));
#13584=CARTESIAN_POINT('Ctrl Pts',(-0.0543213285795041,0.136154072578339,
0.349455397402319));
#13585=CARTESIAN_POINT('Ctrl Pts',(-0.0993361893261098,0.11819451400421,
0.352102786776579));
#13586=CARTESIAN_POINT('Ctrl Pts',(-0.134562512850926,0.0757004080951257,
0.35475017615084));
#13587=CARTESIAN_POINT('Ctrl Pts',(-0.143864833510727,0.0281362381501331,
0.3573975655251));
#13588=CARTESIAN_POINT('Ctrl Pts',(-0.145664973529558,0.0189318504589563,
0.357909875488637));
#13589=CARTESIAN_POINT('Ctrl Pts',(-0.146494308508217,0.00953759842677947,
0.358422185452174));
#13590=CARTESIAN_POINT('Ctrl Pts',(-0.146408012399712,0.000128195943346294,
0.358934495415711));
#13591=CARTESIAN_POINT('Origin',(0.,0.,0.));
#13592=CARTESIAN_POINT('',(-0.146110491840834,1.12683595067248E-5,0.416065504584291));
#13593=CARTESIAN_POINT('',(-0.146109756335714,8.81622270207575E-6,0.40893449541571));
#13594=CARTESIAN_POINT('',(-0.14635,-1.79227059055215E-17,0.));
#13595=CARTESIAN_POINT('Ctrl Pts',(-0.146110491840834,1.12683595067248E-5,
0.416065504584291));
#13596=CARTESIAN_POINT('Ctrl Pts',(-0.146126798292857,0.0237518011834032,
0.414779555213666));
#13597=CARTESIAN_POINT('Ctrl Pts',(-0.140669750958991,0.0474852665485293,
0.413493605843041));
#13598=CARTESIAN_POINT('Ctrl Pts',(-0.129698698951591,0.0683144158983218,
0.412207656472415));
#13599=CARTESIAN_POINT('Ctrl Pts',(-0.107121587134001,0.111178312051432,
0.409561326593314));
#13600=CARTESIAN_POINT('Ctrl Pts',(-0.0611933749717542,0.141742803557285,
0.406914996714211));
#13601=CARTESIAN_POINT('Ctrl Pts',(-0.0129361277491455,0.146018041789781,
0.40426866683511));
#13602=CARTESIAN_POINT('Ctrl Pts',(0.0353211194734639,0.150293280022276,
0.401622336956008));
#13603=CARTESIAN_POINT('Ctrl Pts',(0.0859074017564354,0.128279264981412,
0.398976007076906));
#13604=CARTESIAN_POINT('Ctrl Pts',(0.115668581836909,0.0900521576926538,
0.396329677197804));
#13605=CARTESIAN_POINT('Ctrl Pts',(0.145429761917382,0.0518250504038959,
0.393683347318702));
#13606=CARTESIAN_POINT('Ctrl Pts',(0.154365839795359,-0.0026151491327561,
0.3910370174396));
#13607=CARTESIAN_POINT('Ctrl Pts',(0.138386632036901,-0.0483503050946702,
0.388390687560498));
#13608=CARTESIAN_POINT('Ctrl Pts',(0.122407424278443,-0.094085461056585,
0.385744357681396));
#13609=CARTESIAN_POINT('Ctrl Pts',(0.0815129308835505,-0.131115573443762,
0.383098027802294));
#13610=CARTESIAN_POINT('Ctrl Pts',(0.0344212048624006,-0.142491377230642,
0.380451697923192));
#13611=CARTESIAN_POINT('Ctrl Pts',(-0.0126705211587486,-0.153867181017521,
0.37780536804409));
#13612=CARTESIAN_POINT('Ctrl Pts',(-0.0659594798061549,-0.139588676204105,
0.375159038164988));
#13613=CARTESIAN_POINT('Ctrl Pts',(-0.101054476324393,-0.106191359083811,
0.372512708285887));
#13614=CARTESIAN_POINT('Ctrl Pts',(-0.129554902927378,-0.0790696072742943,
0.370363640385355));
#13615=CARTESIAN_POINT('Ctrl Pts',(-0.146056480184715,-0.0393390709180539,
0.368214572484823));
#13616=CARTESIAN_POINT('Ctrl Pts',(-0.146416087288192,0.000126442170093593,
0.366065504584291));
#13617=CARTESIAN_POINT('Ctrl Pts',(-0.146408012399712,0.000128195943346294,
0.358934495415711));
#13618=CARTESIAN_POINT('Ctrl Pts',(-0.146048368712081,-0.0390859965171687,
0.361069574826434));
#13619=CARTESIAN_POINT('Ctrl Pts',(-0.1297855810823,-0.0785633296797545,
0.363204654237157));
#13620=CARTESIAN_POINT('Ctrl Pts',(-0.101613371150224,-0.105657280969165,
0.36533973364788));
#13621=CARTESIAN_POINT('Ctrl Pts',(-0.066681270335132,-0.139252396162569,
0.36798712302214));
#13622=CARTESIAN_POINT('Ctrl Pts',(-0.0134387509101597,-0.153808392568477,
0.370634512396399));
#13623=CARTESIAN_POINT('Ctrl Pts',(0.0337263783221333,-0.142657876135818,
0.373281901770659));
#13624=CARTESIAN_POINT('Ctrl Pts',(0.0808915075544263,-0.13150735970316,
0.375929291144919));
#13625=CARTESIAN_POINT('Ctrl Pts',(0.12197924659404,-0.0946503304319347,
0.378576680519179));
#13626=CARTESIAN_POINT('Ctrl Pts',(0.138169300408926,-0.0489692009616054,
0.38122406989344));
#13627=CARTESIAN_POINT('Ctrl Pts',(0.154359354223812,-0.00328807149127619,
0.3838714592677));
#13628=CARTESIAN_POINT('Ctrl Pts',(0.14565172281397,0.0512171581781573,
0.38651884864196));
#13629=CARTESIAN_POINT('Ctrl Pts',(0.11603494864959,0.0895802930905963,
0.38916623801622));
#13630=CARTESIAN_POINT('Ctrl Pts',(0.0864181744852101,0.127943428003035,
0.39181362739048));
#13631=CARTESIAN_POINT('Ctrl Pts',(0.0358922575662923,0.15016446815848,
0.394461016764739));
#13632=CARTESIAN_POINT('Ctrl Pts',(-0.0123993367959677,0.146065035738641,
0.397108406138999));
#13633=CARTESIAN_POINT('Ctrl Pts',(-0.0606909311582276,0.141965603318802,
0.399755795513259));
#13634=CARTESIAN_POINT('Ctrl Pts',(-0.106748202963829,0.111545698323679,
0.40240318488752));
#13635=CARTESIAN_POINT('Ctrl Pts',(-0.129474555904152,0.0687391998188283,
0.40505057426178));
#13636=CARTESIAN_POINT('Ctrl Pts',(-0.140588317483115,0.0478057390183907,
0.406345214646423));
#13637=CARTESIAN_POINT('Ctrl Pts',(-0.146122589096428,0.0239100770892618,
0.407639855031067));
#13638=CARTESIAN_POINT('Ctrl Pts',(-0.146109756335714,8.81622270207575E-6,
0.40893449541571));
#13639=CARTESIAN_POINT('Origin',(0.,0.,0.));
#13640=CARTESIAN_POINT('',(-0.146374718215768,-0.000132229735885947,0.466065504584291));
#13641=CARTESIAN_POINT('',(-0.146375609273197,-0.000132432188538665,0.458934495415711));
#13642=CARTESIAN_POINT('',(-0.14635,-1.79227059055215E-17,0.));
#13643=CARTESIAN_POINT('Ctrl Pts',(-0.146374718215768,-0.000132229735885947,
0.466065504584291));
#13644=CARTESIAN_POINT('Ctrl Pts',(-0.146022504084922,0.0379941335185874,
0.46399086782161));
#13645=CARTESIAN_POINT('Ctrl Pts',(-0.130761950520226,0.0763703265456945,
0.46191623105893));
#13646=CARTESIAN_POINT('Ctrl Pts',(-0.103994021541854,0.103314352404769,
0.45984159429625));
#13647=CARTESIAN_POINT('Ctrl Pts',(-0.0698498419286355,0.137683154682254,
0.457195264417148));
#13648=CARTESIAN_POINT('Ctrl Pts',(-0.0169824611430249,0.153451124186949,
0.454548934538046));
#13649=CARTESIAN_POINT('Ctrl Pts',(0.030409888879481,0.143401013202843,
0.451902604658944));
#13650=CARTESIAN_POINT('Ctrl Pts',(0.0778022389019875,0.133350902218736,
0.449256274779842));
#13651=CARTESIAN_POINT('Ctrl Pts',(0.119719558161389,0.0974827107458278,
0.44660994490074));
#13652=CARTESIAN_POINT('Ctrl Pts',(0.136975630157447,0.0522138743269898,
0.443963615021638));
#13653=CARTESIAN_POINT('Ctrl Pts',(0.154231702153504,0.00694503790815254,
0.441317285142536));
#13654=CARTESIAN_POINT('Ctrl Pts',(0.146826526886218,-0.0477244434566137,
0.438670955263434));
#13655=CARTESIAN_POINT('Ctrl Pts',(0.118149569579287,-0.0867714880447125,
0.436024625384332));
#13656=CARTESIAN_POINT('Ctrl Pts',(0.0894726122723542,-0.125818532632812,
0.43337829550523));
#13657=CARTESIAN_POINT('Ctrl Pts',(0.0395238729257754,-0.149243140444243,
0.430731965626129));
#13658=CARTESIAN_POINT('Ctrl Pts',(-0.00883432462988853,-0.146323499949933,
0.428085635747027));
#13659=CARTESIAN_POINT('Ctrl Pts',(-0.0571925221855517,-0.143403859455623,
0.425439305867925));
#13660=CARTESIAN_POINT('Ctrl Pts',(-0.1039601779503,-0.114139970655572,
0.422792975988823));
#13661=CARTESIAN_POINT('Ctrl Pts',(-0.127731000096207,-0.0719263758553634,
0.420146646109721));
#13662=CARTESIAN_POINT('Ctrl Pts',(-0.139950702323481,-0.0502259249733931,
0.418786265601244));
#13663=CARTESIAN_POINT('Ctrl Pts',(-0.146093241566443,-0.0251033736724598,
0.417425885092767));
#13664=CARTESIAN_POINT('Ctrl Pts',(-0.146110491840834,1.12683595067248E-5,
0.416065504584291));
#13665=CARTESIAN_POINT('Ctrl Pts',(-0.146109756335714,8.81622270207575E-6,
0.40893449541571));
#13666=CARTESIAN_POINT('Ctrl Pts',(-0.146096347589706,-0.0249652282079418,
0.410287244405327));
#13667=CARTESIAN_POINT('Ctrl Pts',(-0.140026707259891,-0.049945385460595,
0.411639993394943));
#13668=CARTESIAN_POINT('Ctrl Pts',(-0.127937780377622,-0.0715588049813403,
0.412992742384559));
#13669=CARTESIAN_POINT('Ctrl Pts',(-0.104279217835726,-0.113857219262079,
0.415640131758819));
#13670=CARTESIAN_POINT('Ctrl Pts',(-0.0575666586768896,-0.14326095580898,
0.41828752113308));
#13671=CARTESIAN_POINT('Ctrl Pts',(-0.00919685447762893,-0.146301592903247,
0.42093491050734));
#13672=CARTESIAN_POINT('Ctrl Pts',(0.039172949721632,-0.149342229997515,
0.4235822998816));
#13673=CARTESIAN_POINT('Ctrl Pts',(0.089199998961318,-0.126019767639148,
0.426229689255859));
#13674=CARTESIAN_POINT('Ctrl Pts',(0.117969334952632,-0.0870170915920772,
0.428877078630119));
#13675=CARTESIAN_POINT('Ctrl Pts',(0.146738670943946,-0.0480144155450057,
0.431524468004379));
#13676=CARTESIAN_POINT('Ctrl Pts',(0.154250293686888,0.00666847419077017,
0.43417185737864));
#13677=CARTESIAN_POINT('Ctrl Pts',(0.137063494116028,0.051984005222912,
0.4368192467529));
#13678=CARTESIAN_POINT('Ctrl Pts',(0.119876694545168,0.0972995362550541,
0.43946663612716));
#13679=CARTESIAN_POINT('Ctrl Pts',(0.0779914726605056,0.133247708583562,
0.442114025501419));
#13680=CARTESIAN_POINT('Ctrl Pts',(0.0305934116013849,0.143362412733947,
0.444761414875679));
#13681=CARTESIAN_POINT('Ctrl Pts',(-0.0168046494577345,0.153477116884331,
0.447408804249939));
#13682=CARTESIAN_POINT('Ctrl Pts',(-0.0697155496913122,0.137758352856595,
0.4500561936242));
#13683=CARTESIAN_POINT('Ctrl Pts',(-0.103903378920715,0.103406122000434,
0.45270358299846));
#13684=CARTESIAN_POINT('Ctrl Pts',(-0.130724942802416,0.0764555792150183,
0.45478055380421));
#13685=CARTESIAN_POINT('Ctrl Pts',(-0.146022533856355,0.0380362146017157,
0.45685752460996));
#13686=CARTESIAN_POINT('Ctrl Pts',(-0.146375609273197,-0.000132432188538665,
0.458934495415711));
#13687=CARTESIAN_POINT('Origin',(0.,0.,0.));
#13688=CARTESIAN_POINT('',(-0.146548608312775,6.99729089778146E-5,0.516065504584291));
#13689=CARTESIAN_POINT('',(-0.146550766805835,6.86360251013434E-5,0.508934495415711));
#13690=CARTESIAN_POINT('',(-0.14635,-1.79227059055215E-17,0.));
#13691=CARTESIAN_POINT('Ctrl Pts',(-0.146548608312775,6.99729089778146E-5,
0.516065504584291));
#13692=CARTESIAN_POINT('Ctrl Pts',(-0.146572081366671,0.00404546554386884,
0.515848510308657));
#13693=CARTESIAN_POINT('Ctrl Pts',(-0.146424333269732,0.00801918670503405,
0.515631516033023));
#13694=CARTESIAN_POINT('Ctrl Pts',(-0.146099725131082,0.0119784074854107,
0.51541452175739));
#13695=CARTESIAN_POINT('Ctrl Pts',(-0.142141002193345,0.06026265009261,
0.512768191878288));
#13696=CARTESIAN_POINT('Ctrl Pts',(-0.111878319621163,0.106390286678145,
0.510121861999186));
#13697=CARTESIAN_POINT('Ctrl Pts',(-0.069163383343408,0.129247972261684,
0.507475532120084));
#13698=CARTESIAN_POINT('Ctrl Pts',(-0.0264484470656534,0.152105657845224,
0.504829202240982));
#13699=CARTESIAN_POINT('Ctrl Pts',(0.0287187429176733,0.151693392426768,
0.50218287236188));
#13700=CARTESIAN_POINT('Ctrl Pts',(0.07108729581893,0.128199876374419,0.499536542482778));
#13701=CARTESIAN_POINT('Ctrl Pts',(0.113455848720186,0.10470636032207,0.496890212603677));
#13702=CARTESIAN_POINT('Ctrl Pts',(0.143025764539373,0.0581315936358261,
0.494243882724575));
#13703=CARTESIAN_POINT('Ctrl Pts',(0.146262427589597,0.00979357977770552,
0.491597552845473));
#13704=CARTESIAN_POINT('Ctrl Pts',(0.149499090639821,-0.0385444340804161,
0.488951222966371));
#13705=CARTESIAN_POINT('Ctrl Pts',(0.126402500921083,-0.0886456951104151,
0.486304893087269));
#13706=CARTESIAN_POINT('Ctrl Pts',(0.087544330920799,-0.117578067907642,
0.483658563208167));
#13707=CARTESIAN_POINT('Ctrl Pts',(0.0486861609205161,-0.146510440704867,
0.481012233329065));
#13708=CARTESIAN_POINT('Ctrl Pts',(-0.00593358936131212,-0.154273925269321,
0.478365903449963));
#13709=CARTESIAN_POINT('Ctrl Pts',(-0.0513146009011563,-0.137315052574797,
0.475719573570861));
#13710=CARTESIAN_POINT('Ctrl Pts',(-0.0966956124410008,-0.120356179880273,
0.473073243691759));
#13711=CARTESIAN_POINT('Ctrl Pts',(-0.132837885238862,-0.078674949926771,
0.470426913812657));
#13712=CARTESIAN_POINT('Ctrl Pts',(-0.14319853241738,-0.0313495174248821,
0.467780583933555));
#13713=CARTESIAN_POINT('Ctrl Pts',(-0.145436768368387,-0.0211256884885646,
0.467208890817134));
#13714=CARTESIAN_POINT('Ctrl Pts',(-0.146471775395962,-0.0106384445195334,
0.466637197700712));
#13715=CARTESIAN_POINT('Ctrl Pts',(-0.146374718215768,-0.000132229735885947,
0.466065504584291));
#13716=CARTESIAN_POINT('Ctrl Pts',(-0.146375609273197,-0.000132432188538665,
0.458934495415711));
#13717=CARTESIAN_POINT('Ctrl Pts',(-0.146472577787773,-0.0106150565970108,
0.45950491398422));
#13718=CARTESIAN_POINT('Ctrl Pts',(-0.145442327125792,-0.021078770125739,
0.46007533255273));
#13719=CARTESIAN_POINT('Ctrl Pts',(-0.143213999951756,-0.0312807998000163,
0.460645751121239));
#13720=CARTESIAN_POINT('Ctrl Pts',(-0.132872033528166,-0.0786297930597184,
0.463293140495499));
#13721=CARTESIAN_POINT('Ctrl Pts',(-0.0967233424557573,-0.120342081894533,
0.465940529869759));
#13722=CARTESIAN_POINT('Ctrl Pts',(-0.0513258840937604,-0.13731129538499,
0.46858791924402));
#13723=CARTESIAN_POINT('Ctrl Pts',(-0.00592842573176499,-0.154280508875447,
0.47123530861828));
#13724=CARTESIAN_POINT('Ctrl Pts',(0.0487177999198187,-0.146506647021548,
0.47388269799254));
#13725=CARTESIAN_POINT('Ctrl Pts',(0.0875820145025328,-0.117550537871965,
0.476530087366799));
#13726=CARTESIAN_POINT('Ctrl Pts',(0.126446229085248,-0.0885944287223814,
0.47917747674106));
#13727=CARTESIAN_POINT('Ctrl Pts',(0.149528432599094,-0.0384560722771122,
0.481824866115319));
#13728=CARTESIAN_POINT('Ctrl Pts',(0.146255790172295,0.0098985887573764,
0.484472255489579));
#13729=CARTESIAN_POINT('Ctrl Pts',(0.142983147745498,0.0582532497918637,
0.487119644863839));
#13730=CARTESIAN_POINT('Ctrl Pts',(0.113355659378058,0.10482421541557,0.4897670342381));
#13731=CARTESIAN_POINT('Ctrl Pts',(0.0709442366160257,0.128279591164298,
0.49241442361236));
#13732=CARTESIAN_POINT('Ctrl Pts',(0.0285328138539934,0.151734966913027,
0.49506181298662));
#13733=CARTESIAN_POINT('Ctrl Pts',(-0.0266625433026316,0.152074752786777,
0.497709202360879));
#13734=CARTESIAN_POINT('Ctrl Pts',(-0.0693595260588707,0.129143309401606,
0.500356591735139));
#13735=CARTESIAN_POINT('Ctrl Pts',(-0.11205650881511,0.106211866016435,
0.503003981109399));
#13736=CARTESIAN_POINT('Ctrl Pts',(-0.142255117170964,0.060009193372344,
0.505651370483659));
#13737=CARTESIAN_POINT('Ctrl Pts',(-0.146122837288996,0.0116984888307781,
0.50829875985792));
#13738=CARTESIAN_POINT('Ctrl Pts',(-0.146432431239741,0.00783142983325791,
0.508510671710517));
#13739=CARTESIAN_POINT('Ctrl Pts',(-0.14657331536999,0.00395086404934249,
0.508722583563114));
#13740=CARTESIAN_POINT('Ctrl Pts',(-0.146550766805835,6.86360251013434E-5,
0.508934495415711));
#13741=CARTESIAN_POINT('Origin',(0.,0.,0.));
#13742=CARTESIAN_POINT('',(-0.146165204287215,8.83645032875094E-5,0.566065504584291));
#13743=CARTESIAN_POINT('',(-0.146168951232552,9.12430751481418E-5,0.558934495415711));
#13744=CARTESIAN_POINT('',(-0.14635,-1.79227059055215E-17,0.));
#13745=CARTESIAN_POINT('Ctrl Pts',(-0.146165204287215,8.83645032875094E-5,
0.566065504584291));
#13746=CARTESIAN_POINT('Ctrl Pts',(-0.146267412293664,0.0186373661349918,
0.565059822916602));
#13747=CARTESIAN_POINT('Ctrl Pts',(-0.142994166834961,0.0371516370495788,
0.564054141248913));
#13748=CARTESIAN_POINT('Ctrl Pts',(-0.136179985035193,0.0542551712289143,
0.563048459581224));
#13749=CARTESIAN_POINT('Ctrl Pts',(-0.118249288396568,0.0992610562830057,
0.560402129702122));
#13750=CARTESIAN_POINT('Ctrl Pts',(-0.0758005933416487,0.134498778989873,
0.55775579982302));
#13751=CARTESIAN_POINT('Ctrl Pts',(-0.0282633354322908,0.143839479279877,
0.555109469943918));
#13752=CARTESIAN_POINT('Ctrl Pts',(0.0192739224770691,0.153180179569881,
0.552463140064816));
#13753=CARTESIAN_POINT('Ctrl Pts',(0.0718997432408687,0.136623857443018,
0.549816810185715));
#13754=CARTESIAN_POINT('Ctrl Pts',(0.105526460745998,0.101748602013432,
0.547170480306613));
#13755=CARTESIAN_POINT('Ctrl Pts',(0.139153178251127,0.0668733465838454,
0.544524150427511));
#13756=CARTESIAN_POINT('Ctrl Pts',(0.153780792497586,0.0136791578515372,
0.541877820548409));
#13757=CARTESIAN_POINT('Ctrl Pts',(0.142714014311998,-0.0334861471092027,
0.539231490669307));
#13758=CARTESIAN_POINT('Ctrl Pts',(0.13164723612641,-0.0806514520699426,
0.536585160790205));
#13759=CARTESIAN_POINT('Ctrl Pts',(0.0948860655087725,-0.121787873259113,
0.533938830911103));
#13760=CARTESIAN_POINT('Ctrl Pts',(0.0492566686055307,-0.138066623508903,
0.531292501032001));
#13761=CARTESIAN_POINT('Ctrl Pts',(0.00362727170228945,-0.154345373758693,
0.528646171152899));
#13762=CARTESIAN_POINT('Ctrl Pts',(-0.050870351486557,-0.145766453069103,
0.525999841273797));
#13763=CARTESIAN_POINT('Ctrl Pts',(-0.089291781429334,-0.116256568409877,
0.523353511394695));
#13764=CARTESIAN_POINT('Ctrl Pts',(-0.124562723435938,-0.0891664410515947,
0.520924175791227));
#13765=CARTESIAN_POINT('Ctrl Pts',(-0.146285818313441,-0.0444372186796531,
0.518494840187759));
#13766=CARTESIAN_POINT('Ctrl Pts',(-0.146548608312775,6.99729089778146E-5,
0.516065504584291));
#13767=CARTESIAN_POINT('Ctrl Pts',(-0.146550766805835,6.86360251013434E-5,
0.508934495415711));
#13768=CARTESIAN_POINT('Ctrl Pts',(-0.146291618860727,-0.0445493453248537,
0.511369972937373));
#13769=CARTESIAN_POINT('Ctrl Pts',(-0.124445252016267,-0.0893868858389474,
0.513805450459036));
#13770=CARTESIAN_POINT('Ctrl Pts',(-0.0890226177929609,-0.116463349340462,
0.516240927980699));
#13771=CARTESIAN_POINT('Ctrl Pts',(-0.0505178462986829,-0.145895746531099,
0.518888317354959));
#13772=CARTESIAN_POINT('Ctrl Pts',(0.00402852857008221,-0.154341804473332,
0.52153570672922));
#13773=CARTESIAN_POINT('Ctrl Pts',(0.0496314652424392,-0.137932794781367,
0.52418309610348));
#13774=CARTESIAN_POINT('Ctrl Pts',(0.0952344019147948,-0.121523785089403,
0.52683048547774));
#13775=CARTESIAN_POINT('Ctrl Pts',(0.131893900390741,-0.0802597077632436,
0.529477874851999));
#13776=CARTESIAN_POINT('Ctrl Pts',(0.14281802728161,-0.0330416298281342,
0.532125264226259));
#13777=CARTESIAN_POINT('Ctrl Pts',(0.153742154172479,0.0141764481069759,
0.53477265360052));
#13778=CARTESIAN_POINT('Ctrl Pts',(0.138930909478268,0.0673485266510362,
0.53742004297478));
#13779=CARTESIAN_POINT('Ctrl Pts',(0.105168604077417,0.102119062543277,
0.54006743234904));
#13780=CARTESIAN_POINT('Ctrl Pts',(0.0714062986765666,0.136889598435517,
0.5427148217233));
#13781=CARTESIAN_POINT('Ctrl Pts',(0.018692932569077,0.153258591675938,
0.545362211097559));
#13782=CARTESIAN_POINT('Ctrl Pts',(-0.0288260648428939,0.143728202535144,
0.548009600471819));
#13783=CARTESIAN_POINT('Ctrl Pts',(-0.0763450622548654,0.13419781339435,
0.550656989846079));
#13784=CARTESIAN_POINT('Ctrl Pts',(-0.118669690971318,0.0987680418723385,
0.55330437922034));
#13785=CARTESIAN_POINT('Ctrl Pts',(-0.136413096952957,0.0536675432455532,
0.5559517685946));
#13786=CARTESIAN_POINT('Ctrl Pts',(-0.143076734904351,0.036729792140314,
0.556946010868304));
#13787=CARTESIAN_POINT('Ctrl Pts',(-0.146273385252938,0.0184280612467595,
0.557940253142007));
#13788=CARTESIAN_POINT('Ctrl Pts',(-0.146168951232552,9.12430751481418E-5,
0.558934495415711));
#13789=CARTESIAN_POINT('Origin',(0.,0.,0.));
#13790=CARTESIAN_POINT('',(-0.146227179098081,-0.000117664897458569,0.616065504584291));
#13791=CARTESIAN_POINT('',(-0.146218520919543,-0.000115076211918358,0.608934495415711));
#13792=CARTESIAN_POINT('',(-0.14635,-1.79227059055215E-17,0.));
#13793=CARTESIAN_POINT('Ctrl Pts',(-0.146227179098081,-0.000117664897458569,
0.616065504584291));
#13794=CARTESIAN_POINT('Ctrl Pts',(-0.145977603365176,0.0329427899635141,
0.614271135524546));
#13795=CARTESIAN_POINT('Ctrl Pts',(-0.134874795495675,0.0661550248562671,
0.612476766464802));
#13796=CARTESIAN_POINT('Ctrl Pts',(-0.114309815624116,0.091770790457776,
0.610682397405058));
#13797=CARTESIAN_POINT('Ctrl Pts',(-0.0839806476072558,0.129548841477563,
0.608036067525956));
#13798=CARTESIAN_POINT('Ctrl Pts',(-0.0330710111925292,0.150804375664025,
0.605389737646855));
#13799=CARTESIAN_POINT('Ctrl Pts',(0.0151169520838501,0.145808400611758,
0.602743407767753));
#13800=CARTESIAN_POINT('Ctrl Pts',(0.0633049153602295,0.140812425559491,
0.600097077888651));
#13801=CARTESIAN_POINT('Ctrl Pts',(0.108771205498262,0.109564941268491,
0.597450748009549));
#13802=CARTESIAN_POINT('Ctrl Pts',(0.130705186191441,0.0663684129079872,
0.594804418130447));
#13803=CARTESIAN_POINT('Ctrl Pts',(0.152639166884621,0.023171884547483,
0.592158088251345));
#13804=CARTESIAN_POINT('Ctrl Pts',(0.151040838132949,-0.0319736878825246,
0.589511758372243));
#13805=CARTESIAN_POINT('Ctrl Pts',(0.126641780152193,-0.0738273082886534,
0.586865428493141));
#13806=CARTESIAN_POINT('Ctrl Pts',(0.102242722171437,-0.115680928694782,
0.584219098614039));
#13807=CARTESIAN_POINT('Ctrl Pts',(0.0550429349615966,-0.14424259707703,
0.581572768734937));
#13808=CARTESIAN_POINT('Ctrl Pts',(0.00664650371163741,-0.14643918846291,
0.578926438855836));
#13809=CARTESIAN_POINT('Ctrl Pts',(-0.0417499275383225,-0.148635779848789,
0.576280108976733));
#13810=CARTESIAN_POINT('Ctrl Pts',(-0.0913430028284016,-0.1244672942383,
0.573633779097631));
#13811=CARTESIAN_POINT('Ctrl Pts',(-0.119433191362276,-0.0849960277323969,
0.570987449218529));
#13812=CARTESIAN_POINT('Ctrl Pts',(-0.136848298201485,-0.0605249807527623,
0.569346801007117));
#13813=CARTESIAN_POINT('Ctrl Pts',(-0.145998464265635,-0.0301720919893573,
0.567706152795704));
#13814=CARTESIAN_POINT('Ctrl Pts',(-0.146165204287215,8.83645032875094E-5,
0.566065504584291));
#13815=CARTESIAN_POINT('Ctrl Pts',(-0.146168951232552,9.12430751481418E-5,
0.558934495415711));
#13816=CARTESIAN_POINT('Ctrl Pts',(-0.145995306636495,-0.0303977620653178,
0.560587642516267));
#13817=CARTESIAN_POINT('Ctrl Pts',(-0.136695352934655,-0.0609837708898569,
0.562240789616823));
#13818=CARTESIAN_POINT('Ctrl Pts',(-0.119031718004195,-0.0855580991331628,
0.563893936717379));
#13819=CARTESIAN_POINT('Ctrl Pts',(-0.090744749826965,-0.124912017153538,
0.566541326091639));
#13820=CARTESIAN_POINT('Ctrl Pts',(-0.0410086302256792,-0.148848627462727,
0.5691887154659));
#13821=CARTESIAN_POINT('Ctrl Pts',(0.00739494322942312,-0.146403732988417,
0.57183610484016));
#13822=CARTESIAN_POINT('Ctrl Pts',(0.0557985166845234,-0.143958838514108,
0.57448349421442));
#13823=CARTESIAN_POINT('Ctrl Pts',(0.10286954399344,-0.1151324392563,0.57713088358868));
#13824=CARTESIAN_POINT('Ctrl Pts',(0.127047076753504,-0.0731285067993286,
0.579778272962939));
#13825=CARTESIAN_POINT('Ctrl Pts',(0.151224609513568,-0.031124574342357,
0.5824256623372));
#13826=CARTESIAN_POINT('Ctrl Pts',(0.15250864772478,0.0240568913137802,
0.58507305171146));
#13827=CARTESIAN_POINT('Ctrl Pts',(0.130311035929276,0.0671399443948921,
0.58772044108572));
#13828=CARTESIAN_POINT('Ctrl Pts',(0.108113424133771,0.110222997476006,
0.59036783045998));
#13829=CARTESIAN_POINT('Ctrl Pts',(0.0624341623315493,0.141207637982093,
0.593015219834239));
#13830=CARTESIAN_POINT('Ctrl Pts',(0.0141966988324609,0.145901308974836,
0.595662609208499));
#13831=CARTESIAN_POINT('Ctrl Pts',(-0.0340407646666261,0.150594979967579,
0.598309998582759));
#13832=CARTESIAN_POINT('Ctrl Pts',(-0.0848364298625779,0.128997681446978,
0.60095738795702));
#13833=CARTESIAN_POINT('Ctrl Pts',(-0.114923272877171,0.091002085522857,
0.60360477733128));
#13834=CARTESIAN_POINT('Ctrl Pts',(-0.135113526827902,0.0655045372973676,
0.60538135002609));
#13835=CARTESIAN_POINT('Ctrl Pts',(-0.14597798884013,0.0326223532682757,
0.6071579227209));
#13836=CARTESIAN_POINT('Ctrl Pts',(-0.146218520919543,-0.000115076211918358,
0.608934495415711));
#13837=CARTESIAN_POINT('Origin',(0.,0.,0.));
#13838=CARTESIAN_POINT('',(-0.146586033401767,-2.15382961294558E-5,0.66606550458429));
#13839=CARTESIAN_POINT('',(-0.146582846697157,-3.00215943766004E-5,0.65893449541571));
#13840=CARTESIAN_POINT('',(-0.14635,-1.79227059055215E-17,0.));
#13841=CARTESIAN_POINT('Ctrl Pts',(-0.146586033401767,-2.15382961294558E-5,
0.66606550458429));
#13842=CARTESIAN_POINT('Ctrl Pts',(-0.146488810225965,0.0472697707580183,
0.663482448132491));
#13843=CARTESIAN_POINT('Ctrl Pts',(-0.121516563758978,0.0946492637554097,
0.660899391680692));
#13844=CARTESIAN_POINT('Ctrl Pts',(-0.0824084263440199,0.121233094478226,
0.658316335228893));
#13845=CARTESIAN_POINT('Ctrl Pts',(-0.0423423130056393,0.148468111155377,
0.655670005349791));
#13846=CARTESIAN_POINT('Ctrl Pts',(0.0125607065496858,0.153876184485078,
0.653023675470689));
#13847=CARTESIAN_POINT('Ctrl Pts',(0.0571706564953393,0.134981954220393,
0.650377345591587));
#13848=CARTESIAN_POINT('Ctrl Pts',(0.101780606440992,0.116087723955709,
0.647731015712485));
#13849=CARTESIAN_POINT('Ctrl Pts',(0.136097486776972,0.0728911900966409,
0.645084685833384));
#13850=CARTESIAN_POINT('Ctrl Pts',(0.144413921474191,0.0251640857912735,
0.642438355954282));
#13851=CARTESIAN_POINT('Ctrl Pts',(0.152730356171409,-0.0225630185140953,
0.63979202607518));
#13852=CARTESIAN_POINT('Ctrl Pts',(0.135046345229863,-0.0748206932657649,
0.637145696196077));
#13853=CARTESIAN_POINT('Ctrl Pts',(0.0994561386758346,-0.10768977857233,
0.634499366316975));
#13854=CARTESIAN_POINT('Ctrl Pts',(0.0638659321218069,-0.140558863878895,
0.631853036437873));
#13855=CARTESIAN_POINT('Ctrl Pts',(0.0103695299552984,-0.154039359740357,
0.629206706558772));
#13856=CARTESIAN_POINT('Ctrl Pts',(-0.0365469229059137,-0.141961031115491,
0.62656037667967));
#13857=CARTESIAN_POINT('Ctrl Pts',(-0.0834633757671259,-0.129882702490626,
0.623914046800568));
#13858=CARTESIAN_POINT('Ctrl Pts',(-0.123799879323041,-0.0922455493794331,
0.621267716921466));
#13859=CARTESIAN_POINT('Ctrl Pts',(-0.139093781291504,-0.0462766888972804,
0.618621387042364));
#13860=CARTESIAN_POINT('Ctrl Pts',(-0.14401750805555,-0.0314774500153124,
0.617769426223006));
#13861=CARTESIAN_POINT('Ctrl Pts',(-0.14634567687575,-0.0158146654998378,
0.616917465403648));
#13862=CARTESIAN_POINT('Ctrl Pts',(-0.146227179098081,-0.000117664897458569,
0.616065504584291));
#13863=CARTESIAN_POINT('Ctrl Pts',(-0.146218520919543,-0.000115076211918358,
0.608934495415711));
#13864=CARTESIAN_POINT('Ctrl Pts',(-0.1463364217222,-0.0161618722236638,
0.60980531209516));
#13865=CARTESIAN_POINT('Ctrl Pts',(-0.143901781624712,-0.032173889023867,
0.61067612877461));
#13866=CARTESIAN_POINT('Ctrl Pts',(-0.138761720114909,-0.0472643972675185,
0.611546945454059));
#13867=CARTESIAN_POINT('Ctrl Pts',(-0.123135303504819,-0.0931413908061287,
0.614194334828319));
#13868=CARTESIAN_POINT('Ctrl Pts',(-0.0825044494514074,-0.130501484555709,
0.616841724202579));
#13869=CARTESIAN_POINT('Ctrl Pts',(-0.0354801761942514,-0.142231836504824,
0.619489113576839));
#13870=CARTESIAN_POINT('Ctrl Pts',(0.0115440970629072,-0.15396218845394,
0.6221365029511));
#13871=CARTESIAN_POINT('Ctrl Pts',(0.0649617895238099,-0.140062798602586,
0.624783892325359));
#13872=CARTESIAN_POINT('Ctrl Pts',(0.100304854137336,-0.106900301471969,
0.627431281699619));
#13873=CARTESIAN_POINT('Ctrl Pts',(0.135647918750861,-0.0737378043413545,
0.630078671073879));
#13874=CARTESIAN_POINT('Ctrl Pts',(0.15291635551701,-0.0213121999314781,
0.63272606044814));
#13875=CARTESIAN_POINT('Ctrl Pts',(0.144200333369931,0.026362891994447,
0.6353734498224));
#13876=CARTESIAN_POINT('Ctrl Pts',(0.135484311222852,0.0740379839203748,
0.63802083919666));
#13877=CARTESIAN_POINT('Ctrl Pts',(0.100783830162543,0.11696256336235,0.640668228570919));
#13878=CARTESIAN_POINT('Ctrl Pts',(0.055993492972559,0.135474968031154,
0.643315617945179));
#13879=CARTESIAN_POINT('Ctrl Pts',(0.0112031557825773,0.153987372699956,
0.64596300731944));
#13880=CARTESIAN_POINT('Ctrl Pts',(-0.04367703753708,0.148087602595587,
0.6486103966937));
#13881=CARTESIAN_POINT('Ctrl Pts',(-0.0835091394177698,0.120478055479053,
0.65125778606796));
#13882=CARTESIAN_POINT('Ctrl Pts',(-0.122009894390588,0.0937913289882395,
0.653816689183877));
#13883=CARTESIAN_POINT('Ctrl Pts',(-0.146451680634158,0.0468218259492564,
0.656375592299793));
#13884=CARTESIAN_POINT('Ctrl Pts',(-0.146582846697157,-3.00215943766004E-5,
0.65893449541571));
#13885=CARTESIAN_POINT('Origin',(0.,0.,0.));
#13886=CARTESIAN_POINT('',(-0.146290249280603,0.000131112932912382,0.716065504584291));
#13887=CARTESIAN_POINT('',(-0.146307221518699,0.000133045872591754,0.708934495415711));
#13888=CARTESIAN_POINT('',(-0.14635,-1.79227059055215E-17,0.));
#13889=CARTESIAN_POINT('Ctrl Pts',(-0.146290249280603,0.000131112932912382,
0.716065504584291));
#13890=CARTESIAN_POINT('Ctrl Pts',(-0.146406294125046,0.0134819654399978,
0.715340090619538));
#13891=CARTESIAN_POINT('Ctrl Pts',(-0.144729088574721,0.0268041890186768,
0.714614676654786));
#13892=CARTESIAN_POINT('Ctrl Pts',(-0.141142411757643,0.0395908011096033,
0.713889262690033));
#13893=CARTESIAN_POINT('Ctrl Pts',(-0.128058117149462,0.0862367098911347,
0.711242932810931));
#13894=CARTESIAN_POINT('Ctrl Pts',(-0.0895623832093418,0.125754646095387,
0.708596602931829));
#13895=CARTESIAN_POINT('Ctrl Pts',(-0.0432753130058998,0.140056628595385,
0.705950273052727));
#13896=CARTESIAN_POINT('Ctrl Pts',(0.00301175719754219,0.154358611095384,
0.703303943173625));
#13897=CARTESIAN_POINT('Ctrl Pts',(0.0570901636643063,0.143444639891129,
0.700657613294523));
#13898=CARTESIAN_POINT('Ctrl Pts',(0.0942073689518517,0.11231021130972,
0.698011283415421));
#13899=CARTESIAN_POINT('Ctrl Pts',(0.131324574239397,0.0811757827283121,
0.695364953536319));
#13900=CARTESIAN_POINT('Ctrl Pts',(0.151480578347723,0.0298208967697505,
0.692718623657217));
#13901=CARTESIAN_POINT('Ctrl Pts',(0.145449661086834,-0.0182485073085286,
0.690072293778115));
#13902=CARTESIAN_POINT('Ctrl Pts',(0.139418743825945,-0.0663179113868083,
0.687425963899014));
#13903=CARTESIAN_POINT('Ctrl Pts',(0.107200905195838,-0.111101833584806,
0.684779634019911));
#13904=CARTESIAN_POINT('Ctrl Pts',(0.0635427568131047,-0.132101968137704,
0.68213330414081));
#13905=CARTESIAN_POINT('Ctrl Pts',(0.0198846084303716,-0.153102102690602,
0.679486974261708));
#13906=CARTESIAN_POINT('Ctrl Pts',(-0.0352138497049885,-0.150318449598402,
0.676840644382606));
#13907=CARTESIAN_POINT('Ctrl Pts',(-0.0765331864534889,-0.125025130675956,
0.674194314503504));
#13908=CARTESIAN_POINT('Ctrl Pts',(-0.117852523201989,-0.0997318117535095,
0.671547984624402));
#13909=CARTESIAN_POINT('Ctrl Pts',(-0.14539273856363,-0.0519288270008166,
0.6689016547453));
#13910=CARTESIAN_POINT('Ctrl Pts',(-0.146548242683733,-0.00349635461217019,
0.666255324866198));
#13911=CARTESIAN_POINT('Ctrl Pts',(-0.146575870647472,-0.00233834005587287,
0.666192051438896));
#13912=CARTESIAN_POINT('Ctrl Pts',(-0.146588414938392,-0.00117996563262623,
0.666128778011593));
#13913=CARTESIAN_POINT('Ctrl Pts',(-0.146586033401767,-2.15382961294558E-5,
0.66606550458429));
#13914=CARTESIAN_POINT('Ctrl Pts',(-0.146582846697157,-3.00215943766004E-5,
0.65893449541571));
#13915=CARTESIAN_POINT('Ctrl Pts',(-0.146587382388275,-0.00165014728799839,
0.659022981674053));
#13916=CARTESIAN_POINT('Ctrl Pts',(-0.146562848415234,-0.00327013229389975,
0.659111467932396));
#13917=CARTESIAN_POINT('Ctrl Pts',(-0.146508820881567,-0.00488913307276392,
0.659199954190739));
#13918=CARTESIAN_POINT('Ctrl Pts',(-0.144892390022949,-0.0533274503793473,
0.661847343564999));
#13919=CARTESIAN_POINT('Ctrl Pts',(-0.116875517863988,-0.100884760863813,
0.66449473293926));
#13920=CARTESIAN_POINT('Ctrl Pts',(-0.0752913709948059,-0.125777373450206,
0.66714212231352));
#13921=CARTESIAN_POINT('Ctrl Pts',(-0.0337072241256252,-0.150669986036599,
0.66978951168778));
#13922=CARTESIAN_POINT('Ctrl Pts',(0.021444197453776,-0.15289790072492,
0.672436901062039));
#13923=CARTESIAN_POINT('Ctrl Pts',(0.0649007096996251,-0.131440618146733,
0.675084290436299));
#13924=CARTESIAN_POINT('Ctrl Pts',(0.108357221945475,-0.109983335568545,
0.677731679810559));
#13925=CARTESIAN_POINT('Ctrl Pts',(0.140118824857774,-0.0648408557238465,
0.68037906918482));
#13926=CARTESIAN_POINT('Ctrl Pts',(0.145637072805965,-0.0166907532130915,
0.68302645855908));
#13927=CARTESIAN_POINT('Ctrl Pts',(0.151155320754156,0.031459349297663,
0.68567384793334));
#13928=CARTESIAN_POINT('Ctrl Pts',(0.130430213738242,0.0826170744744734,
0.688321237307599));
#13929=CARTESIAN_POINT('Ctrl Pts',(0.0929549153570804,0.113349556369966,
0.690968626681859));
#13930=CARTESIAN_POINT('Ctrl Pts',(0.0554796169759186,0.14408203826546,
0.693616016056119));
#13931=CARTESIAN_POINT('Ctrl Pts',(0.00125412722950909,0.154389276879634,
0.69626340543038));
#13932=CARTESIAN_POINT('Ctrl Pts',(-0.0448834941801804,0.139550027475769,
0.69891079480464));
#13933=CARTESIAN_POINT('Ctrl Pts',(-0.0910211155898686,0.124710778071904,
0.7015581841789));
#13934=CARTESIAN_POINT('Ctrl Pts',(-0.129070868662838,0.0847250406500019,
0.704205573553159));
#13935=CARTESIAN_POINT('Ctrl Pts',(-0.141604011991841,0.0379083368947344,
0.706852962927419));
#13936=CARTESIAN_POINT('Ctrl Pts',(-0.144888775625201,0.0256383259412015,
0.707546807090183));
#13937=CARTESIAN_POINT('Ctrl Pts',(-0.146420824649375,0.0128991016161637,
0.708240651252947));
#13938=CARTESIAN_POINT('Ctrl Pts',(-0.146307221518699,0.000133045872591754,
0.708934495415711));
#13939=CARTESIAN_POINT('Origin',(0.,0.,0.));
#13940=CARTESIAN_POINT('',(-0.1461301977291,-5.61458017395017E-5,0.766065504584291));
#13941=CARTESIAN_POINT('',(-0.14612241379348,-4.54149644099216E-5,0.758934495415711));
#13942=CARTESIAN_POINT('',(-0.14635,-1.79227059055215E-17,0.));
#13943=CARTESIAN_POINT('Ctrl Pts',(-0.1461301977291,-5.61458017395017E-5,
0.766065504584291));
#13944=CARTESIAN_POINT('Ctrl Pts',(-0.14603380141711,0.0278870014676159,
0.764551403227483));
#13945=CARTESIAN_POINT('Ctrl Pts',(-0.138327245009168,0.0558793842949389,
0.763037301870675));
#13946=CARTESIAN_POINT('Ctrl Pts',(-0.123350675409043,0.079203679241543,
0.761523200513867));
#13947=CARTESIAN_POINT('Ctrl Pts',(-0.0971747899961838,0.119969628197767,
0.758876870634766));
#13948=CARTESIAN_POINT('Ctrl Pts',(-0.048790709571801,0.146475657227381,
0.756230540755664));
#13949=CARTESIAN_POINT('Ctrl Pts',(-0.000344588961360588,0.146589539830481,
0.753584210876561));
#13950=CARTESIAN_POINT('Ctrl Pts',(0.0481015316490792,0.14670342243358,
0.750937880997459));
#13951=CARTESIAN_POINT('Ctrl Pts',(0.0966096924455767,0.120425158610167,
0.748291551118357));
#13952=CARTESIAN_POINT('Ctrl Pts',(0.122976945064223,0.0797827231418903,
0.745645221239255));
#13953=CARTESIAN_POINT('Ctrl Pts',(0.149344197682869,0.0391402876736125,
0.742998891360154));
#13954=CARTESIAN_POINT('Ctrl Pts',(0.153570542123663,-0.01586631943953,
0.740352561481052));
#13955=CARTESIAN_POINT('Ctrl Pts',(0.133721514043982,-0.0600597087159893,
0.73770623160195));
#13956=CARTESIAN_POINT('Ctrl Pts',(0.113872485964301,-0.104253097992448,
0.735059901722848));
#13957=CARTESIAN_POINT('Ctrl Pts',(0.0699480853641458,-0.137633269432224,
0.732413571843746));
#13958=CARTESIAN_POINT('Ctrl Pts',(0.0220532014503509,-0.144921593405036,
0.729767241964644));
#13959=CARTESIAN_POINT('Ctrl Pts',(-0.0258416824634434,-0.152209917377848,
0.727120912085542));
#13960=CARTESIAN_POINT('Ctrl Pts',(-0.0777070496908773,-0.133406393883698,
0.724474582206441));
#13961=CARTESIAN_POINT('Ctrl Pts',(-0.109803305666473,-0.0971176914572187,
0.721828252327339));
#13962=CARTESIAN_POINT('Ctrl Pts',(-0.133101311474982,-0.0707764758164216,
0.71990733641299));
#13963=CARTESIAN_POINT('Ctrl Pts',(-0.14598295937539,-0.0352223077304616,
0.71798642049864));
#13964=CARTESIAN_POINT('Ctrl Pts',(-0.146290249280603,0.000131112932912382,
0.716065504584291));
#13965=CARTESIAN_POINT('Ctrl Pts',(-0.146307221518699,0.000133045872591754,
0.708934495415711));
#13966=CARTESIAN_POINT('Ctrl Pts',(-0.145987367488279,-0.0358102803178394,
0.710888040627207));
#13967=CARTESIAN_POINT('Ctrl Pts',(-0.132622002370819,-0.0719663061161047,
0.712841585838703));
#13968=CARTESIAN_POINT('Ctrl Pts',(-0.1086007072861,-0.0984612847532928,
0.7147951310502));
#13969=CARTESIAN_POINT('Ctrl Pts',(-0.0760477256663158,-0.134366532557423,
0.71744252042446));
#13970=CARTESIAN_POINT('Ctrl Pts',(-0.0239252288417074,-0.152529358077047,
0.720089909798719));
#13971=CARTESIAN_POINT('Ctrl Pts',(0.0238920022682765,-0.144630254255197,
0.722737299172979));
#13972=CARTESIAN_POINT('Ctrl Pts',(0.071709233378259,-0.136731150433346,
0.725384688547239));
#13973=CARTESIAN_POINT('Ctrl Pts',(0.115221198773618,-0.102770117270024,
0.7280320779215));
#13974=CARTESIAN_POINT('Ctrl Pts',(0.134497183226257,-0.058303052428779,
0.730679467295759));
#13975=CARTESIAN_POINT('Ctrl Pts',(0.153773167678896,-0.0138359875875333,
0.733326856670019));
#13976=CARTESIAN_POINT('Ctrl Pts',(0.148813171188813,0.0411371089316358,
0.735974246044279));
#13977=CARTESIAN_POINT('Ctrl Pts',(0.121889126928366,0.0814357351225549,
0.738621635418539));
#13978=CARTESIAN_POINT('Ctrl Pts',(0.0949650826679194,0.121734361313473,
0.741269024792799));
#13979=CARTESIAN_POINT('Ctrl Pts',(0.0460769906371109,0.147358517176143,
0.74391641416706));
#13980=CARTESIAN_POINT('Ctrl Pts',(-0.00238189178169058,0.146571023090686,
0.74656380354132));
#13981=CARTESIAN_POINT('Ctrl Pts',(-0.0508407742004934,0.14578352900523,
0.74921119291558));
#13982=CARTESIAN_POINT('Ctrl Pts',(-0.0988704470072894,0.118584384971644,
0.751858582289839));
#13983=CARTESIAN_POINT('Ctrl Pts',(-0.124470852918682,0.0774321960944291,
0.754505971664099));
#13984=CARTESIAN_POINT('Ctrl Pts',(-0.138745545153454,0.0544858868428234,
0.75598214624797));
#13985=CARTESIAN_POINT('Ctrl Pts',(-0.146046671909043,0.027201385339783,
0.757458320831841));
#13986=CARTESIAN_POINT('Ctrl Pts',(-0.14612241379348,-4.54149644099216E-5,
0.758934495415711));
#13987=CARTESIAN_POINT('Origin',(0.,0.,0.));
#13988=CARTESIAN_POINT('',(-0.146495788566881,-0.000101744904923998,0.816065504584291));
#13989=CARTESIAN_POINT('',(-0.146473871348434,-0.000110945968026819,0.808934495415711));
#13990=CARTESIAN_POINT('',(-0.14635,-1.79227059055215E-17,0.));
#13991=CARTESIAN_POINT('Ctrl Pts',(-0.146495788566881,-0.000101744904923998,
0.816065504584291));
#13992=CARTESIAN_POINT('Ctrl Pts',(-0.14616118452328,0.0421270051992108,
0.813762715835428));
#13993=CARTESIAN_POINT('Ctrl Pts',(-0.126905337350145,0.0846218946815527,
0.811459927086565));
#13994=CARTESIAN_POINT('Ctrl Pts',(-0.0947343415465314,0.111866064832055,
0.809157138337701));
#13995=CARTESIAN_POINT('Ctrl Pts',(-0.0577639214515077,0.143174651664521,
0.806510808458599));
#13996=CARTESIAN_POINT('Ctrl Pts',(-0.00373742343573488,0.154342745753647,
0.803864478579497));
#13997=CARTESIAN_POINT('Ctrl Pts',(0.0426163743729279,0.140258534729872,
0.801218148700395));
#13998=CARTESIAN_POINT('Ctrl Pts',(0.0889701721815907,0.126174323706097,
0.798571818821294));
#13999=CARTESIAN_POINT('Ctrl Pts',(0.127651269783143,0.0868378075694234,
0.795925488942192));
#14000=CARTESIAN_POINT('Ctrl Pts',(0.140954720244851,0.040253928627653,
0.79327915906309));
#14001=CARTESIAN_POINT('Ctrl Pts',(0.154258170706558,-0.00632995031411615,
0.790632829183988));
#14002=CARTESIAN_POINT('Ctrl Pts',(0.14218397402842,-0.060161192060982,
0.787986499304886));
#14003=CARTESIAN_POINT('Ctrl Pts',(0.110258679990485,-0.0966003903512828,
0.785340169425784));
#14004=CARTESIAN_POINT('Ctrl Pts',(0.0783333859525485,-0.133039588641585,
0.782693839546682));
#14005=CARTESIAN_POINT('Ctrl Pts',(0.0265569945548152,-0.152086743475322,
0.780047509667581));
#14006=CARTESIAN_POINT('Ctrl Pts',(-0.021371625274328,-0.14502367242074,
0.777401179788479));
#14007=CARTESIAN_POINT('Ctrl Pts',(-0.0693002451034712,-0.137960601366157,
0.774754849909377));
#14008=CARTESIAN_POINT('Ctrl Pts',(-0.113381093364023,-0.104787304423254,
0.772108520030274));
#14009=CARTESIAN_POINT('Ctrl Pts',(-0.133437672293631,-0.0606877215103841,
0.769462190151172));
#14010=CARTESIAN_POINT('Ctrl Pts',(-0.1420188514214,-0.0418197768941368,
0.768329961628878));
#14011=CARTESIAN_POINT('Ctrl Pts',(-0.146202281842484,-0.0209517273285418,
0.767197733106584));
#14012=CARTESIAN_POINT('Ctrl Pts',(-0.1461301977291,-5.61458017395017E-5,
0.766065504584291));
#14013=CARTESIAN_POINT('Ctrl Pts',(-0.14612241379348,-4.54149644099216E-5,
0.758934495415711));
#14014=CARTESIAN_POINT('Ctrl Pts',(-0.146182508321779,-0.0216633562673834,
0.760105710206101));
#14015=CARTESIAN_POINT('Ctrl Pts',(-0.141694203021096,-0.0432575645610501,
0.76127692499649));
#14016=CARTESIAN_POINT('Ctrl Pts',(-0.132531725405586,-0.0626424774360703,
0.76244813978688));
#14017=CARTESIAN_POINT('Ctrl Pts',(-0.111821052965107,-0.106459728368519,
0.76509552916114));
#14018=CARTESIAN_POINT('Ctrl Pts',(-0.067228569068158,-0.138988996512573,
0.767742918535399));
#14019=CARTESIAN_POINT('Ctrl Pts',(-0.0191799219195066,-0.145330206128911,
0.770390307909659));
#14020=CARTESIAN_POINT('Ctrl Pts',(0.0288687252291434,-0.151671415745249,
0.773037697283919));
#14021=CARTESIAN_POINT('Ctrl Pts',(0.080373535629496,-0.131824566833873,
0.77568508665818));
#14022=CARTESIAN_POINT('Ctrl Pts',(0.111742660473083,-0.0948805356683208,
0.77833247603244));
#14023=CARTESIAN_POINT('Ctrl Pts',(0.14311178531667,-0.0579365045027684,
0.7809798654067));
#14024=CARTESIAN_POINT('Ctrl Pts',(0.154345224603492,-0.00389529108304171,
0.783627254780959));
#14025=CARTESIAN_POINT('Ctrl Pts',(0.140297486112651,0.0424894529122293,
0.786274644155219));
#14026=CARTESIAN_POINT('Ctrl Pts',(0.126249747621811,0.0888741969075009,
0.788922033529479));
#14027=CARTESIAN_POINT('Ctrl Pts',(0.0869208313533056,0.127602471478316,
0.79156942290374));
#14028=CARTESIAN_POINT('Ctrl Pts',(0.0403254011646538,0.140934737517831,
0.794216812278));
#14029=CARTESIAN_POINT('Ctrl Pts',(-0.00627002902399674,0.154267003557346,
0.79686420165226));
#14030=CARTESIAN_POINT('Ctrl Pts',(-0.0601319731327944,0.142203261065564,
0.799511591026519));
#14031=CARTESIAN_POINT('Ctrl Pts',(-0.0965888940360299,0.110269323781398,
0.802158980400779));
#14032=CARTESIAN_POINT('Ctrl Pts',(-0.127690529151203,0.0830262752573849,
0.804417485405756));
#14033=CARTESIAN_POINT('Ctrl Pts',(-0.146124951115714,0.0413218847513699,
0.806675990410734));
#14034=CARTESIAN_POINT('Ctrl Pts',(-0.146473871348434,-0.000110945968026819,
0.808934495415711));
#14035=CARTESIAN_POINT('Origin',(0.,0.,0.));
#14036=CARTESIAN_POINT('',(-0.146444331750498,0.000119944961782359,0.866065504584291));
#14037=CARTESIAN_POINT('',(-0.146471560192382,0.00011177640072981,0.858934495415711));
#14038=CARTESIAN_POINT('',(-0.14635,-1.79227059055215E-17,0.));
#14039=CARTESIAN_POINT('Ctrl Pts',(-0.146444331750498,0.000119944961782359,
0.866065504584291));
#14040=CARTESIAN_POINT('Ctrl Pts',(-0.146516681599632,0.00829054204730037,
0.865620358322474));
#14041=CARTESIAN_POINT('Ctrl Pts',(-0.145891801779796,0.0164500693154795,
0.865175212060658));
#14042=CARTESIAN_POINT('Ctrl Pts',(-0.14453063157077,0.0244848619971339,
0.864730065798841));
#14043=CARTESIAN_POINT('Ctrl Pts',(-0.136438672357208,0.0722505376181754,
0.862083735919739));
#14044=CARTESIAN_POINT('Ctrl Pts',(-0.102325254887189,0.115607931012472,
0.859437406040638));
#14045=CARTESIAN_POINT('Ctrl Pts',(-0.0578046270350215,0.134711681091902,
0.856791076161536));
#14046=CARTESIAN_POINT('Ctrl Pts',(-0.0132839991828526,0.153815431171333,
0.854144746282434));
#14047=CARTESIAN_POINT('Ctrl Pts',(0.0416438390514653,0.148665537935894,
0.851498416403331));
#14048=CARTESIAN_POINT('Ctrl Pts',(0.081837551941475,0.121619188541491,
0.848852086524229));
#14049=CARTESIAN_POINT('Ctrl Pts',(0.122031264831484,0.0945728391470885,
0.846205756645128));
#14050=CARTESIAN_POINT('Ctrl Pts',(0.147490852377186,0.0456300335937214,
0.843559426766026));
#14051=CARTESIAN_POINT('Ctrl Pts',(0.146563060809277,-0.0028073360113171,
0.840913096886925));
#14052=CARTESIAN_POINT('Ctrl Pts',(0.145635269241369,-0.0512447056163556,
0.838266767007823));
#14053=CARTESIAN_POINT('Ctrl Pts',(0.118320098559852,-0.0991766392730661,
0.835620437128721));
#14054=CARTESIAN_POINT('Ctrl Pts',(0.0771201321287374,-0.124663936845065,
0.832974107249619));
#14055=CARTESIAN_POINT('Ctrl Pts',(0.035920165697623,-0.150151234417064,
0.830327777370517));
#14056=CARTESIAN_POINT('Ctrl Pts',(-0.0191645964830881,-0.153193895904352,
0.827681447491415));
#14057=CARTESIAN_POINT('Ctrl Pts',(-0.0629209921278279,-0.132399247274726,
0.825035117612313));
#14058=CARTESIAN_POINT('Ctrl Pts',(-0.106677387772568,-0.111604598645101,
0.822388787733211));
#14059=CARTESIAN_POINT('Ctrl Pts',(-0.139105416881337,-0.0669726398985626,
0.819742457854109));
#14060=CARTESIAN_POINT('Ctrl Pts',(-0.145362260348583,-0.0189321207373897,
0.817096127975007));
#14061=CARTESIAN_POINT('Ctrl Pts',(-0.146174510965348,-0.0126955988357878,
0.816752586844768));
#14062=CARTESIAN_POINT('Ctrl Pts',(-0.146545706411658,-0.00640163348415362,
0.81640904571453));
#14063=CARTESIAN_POINT('Ctrl Pts',(-0.146495788566881,-0.000101744904923998,
0.816065504584291));
#14064=CARTESIAN_POINT('Ctrl Pts',(-0.146473871348434,-0.000110945968026819,
0.808934495415711));
#14065=CARTESIAN_POINT('Ctrl Pts',(-0.146533950748007,-0.00724512552769256,
0.809323379784994));
#14066=CARTESIAN_POINT('Ctrl Pts',(-0.146057826922151,-0.0143712538186879,
0.809712264154277));
#14067=CARTESIAN_POINT('Ctrl Pts',(-0.145017839345608,-0.0214141189368497,
0.81010114852356));
#14068=CARTESIAN_POINT('Ctrl Pts',(-0.137937966054276,-0.0693594922943736,
0.81274853789782));
#14069=CARTESIAN_POINT('Ctrl Pts',(-0.104726321773939,-0.113446106932874,
0.81539592727208));
#14070=CARTESIAN_POINT('Ctrl Pts',(-0.0605955455659204,-0.133480028752914,
0.818043316646339));
#14071=CARTESIAN_POINT('Ctrl Pts',(-0.0164647693578984,-0.153513950572954,
0.820690706020599));
#14072=CARTESIAN_POINT('Ctrl Pts',(0.0385851387778066,-0.149495179574532,
0.823338095394859));
#14073=CARTESIAN_POINT('Ctrl Pts',(0.0793384931690736,-0.12326451930694,
0.825985484769119));
#14074=CARTESIAN_POINT('Ctrl Pts',(0.120091847560339,-0.0970338590393495,
0.828632874143379));
#14075=CARTESIAN_POINT('Ctrl Pts',(0.146548648207165,-0.0485913095025905,
0.83128026351764));
#14076=CARTESIAN_POINT('Ctrl Pts',(0.146590321408106,-0.000126046730599388,
0.833927652891899));
#14077=CARTESIAN_POINT('Ctrl Pts',(0.146631994609047,0.0483392160413931,
0.836575042266159));
#14078=CARTESIAN_POINT('Ctrl Pts',(0.120258540364101,0.0968271920486179,
0.839222431640419));
#14079=CARTESIAN_POINT('Ctrl Pts',(0.0795503554414038,0.123127897600245,
0.841869821014679));
#14080=CARTESIAN_POINT('Ctrl Pts',(0.0388421705187073,0.149428603151872,
0.844517210388939));
#14081=CARTESIAN_POINT('Ctrl Pts',(-0.0162007450817403,0.153542038247903,
0.8471645997632));
#14082=CARTESIAN_POINT('Ctrl Pts',(-0.0603659086281491,0.133584038319734,
0.84981198913746));
#14083=CARTESIAN_POINT('Ctrl Pts',(-0.104531072174558,0.113626038391565,
0.85245937851172));
#14084=CARTESIAN_POINT('Ctrl Pts',(-0.137818483666928,0.0695966034391962,
0.855106767885979));
#14085=CARTESIAN_POINT('Ctrl Pts',(-0.144980798768897,0.0216634763286692,
0.857754157260239));
#14086=CARTESIAN_POINT('Ctrl Pts',(-0.146045237806912,0.0145398171508471,
0.858147603312063));
#14087=CARTESIAN_POINT('Ctrl Pts',(-0.146532654486068,0.00732993751956911,
0.858541049363887));
#14088=CARTESIAN_POINT('Ctrl Pts',(-0.146471560192382,0.00011177640072981,
0.858934495415711));
#14089=CARTESIAN_POINT('Origin',(0.,0.,0.));
#14090=CARTESIAN_POINT('',(-0.146114231148477,2.69008449349656E-5,0.916065504584291));
#14091=CARTESIAN_POINT('',(-0.146121644853617,4.41067432152685E-5,0.908934495415711));
#14092=CARTESIAN_POINT('',(-0.14635,-1.79227059055215E-17,0.));
#14093=CARTESIAN_POINT('Ctrl Pts',(-0.146114231148477,2.69008449349656E-5,
0.916065504584291));
#14094=CARTESIAN_POINT('Ctrl Pts',(-0.146151635159142,0.0228038459942234,
0.914831670930419));
#14095=CARTESIAN_POINT('Ctrl Pts',(-0.141147538069067,0.0455652341090756,
0.913597837276548));
#14096=CARTESIAN_POINT('Ctrl Pts',(-0.131015765267123,0.0657531838068269,
0.912364003622676));
#14097=CARTESIAN_POINT('Ctrl Pts',(-0.109285110563454,0.109052354902802,
0.909717673743574));
#14098=CARTESIAN_POINT('Ctrl Pts',(-0.0639662294071284,0.140513248471977,
0.907071343864472));
#14099=CARTESIAN_POINT('Ctrl Pts',(-0.015802286694576,0.145735718560985,
0.90442501398537));
#14100=CARTESIAN_POINT('Ctrl Pts',(0.0323616560179757,0.150958188649994,
0.901778684106268));
#14101=CARTESIAN_POINT('Ctrl Pts',(0.0833706602867547,0.129942235258839,
0.899132354227166));
#14102=CARTESIAN_POINT('Ctrl Pts',(0.113877102345416,0.0923071908936453,
0.896486024348064));
#14103=CARTESIAN_POINT('Ctrl Pts',(0.144383544404078,0.0546721465284523,
0.893839694468962));
#14104=CARTESIAN_POINT('Ctrl Pts',(0.15438742425262,0.000418011189221586,
0.891193364589861));
#14105=CARTESIAN_POINT('Ctrl Pts',(0.139309808695705,-0.0456222438118789,
0.888547034710759));
#14106=CARTESIAN_POINT('Ctrl Pts',(0.124232193138789,-0.0916624988129813,
0.885900704831657));
#14107=CARTESIAN_POINT('Ctrl Pts',(0.0840730821764119,-0.129488873475953,
0.883254374952555));
#14108=CARTESIAN_POINT('Ctrl Pts',(0.0372139327097935,-0.141787641004198,
0.880608045073453));
#14109=CARTESIAN_POINT('Ctrl Pts',(-0.00964521675682358,-0.154086408532443,
0.877961715194351));
#14110=CARTESIAN_POINT('Ctrl Pts',(-0.0632044047276821,-0.140857568925962,
0.875315385315249));
#14111=CARTESIAN_POINT('Ctrl Pts',(-0.0989487482345592,-0.108156170198829,
0.872669055436147));
#14112=CARTESIAN_POINT('Ctrl Pts',(-0.128680439645858,-0.0809555616469925,
0.870467871818862));
#14113=CARTESIAN_POINT('Ctrl Pts',(-0.146086572253705,-0.0402824710322022,
0.868266688201576));
#14114=CARTESIAN_POINT('Ctrl Pts',(-0.146444331750498,0.000119944961782359,
0.866065504584291));
#14115=CARTESIAN_POINT('Ctrl Pts',(-0.146471560192382,0.00011177640072981,
0.858934495415711));
#14116=CARTESIAN_POINT('Ctrl Pts',(-0.146121567926216,-0.0412390669452651,
0.861188438738147));
#14117=CARTESIAN_POINT('Ctrl Pts',(-0.127770397964496,-0.0828616943330661,
0.863442382060584));
#14118=CARTESIAN_POINT('Ctrl Pts',(-0.096778382793969,-0.110103055552942,
0.86569632538302));
#14119=CARTESIAN_POINT('Ctrl Pts',(-0.0603764330055066,-0.142099641055337,
0.86834371475728));
#14120=CARTESIAN_POINT('Ctrl Pts',(-0.00653531471701479,-0.154255992791443,
0.870991104131539));
#14121=CARTESIAN_POINT('Ctrl Pts',(0.040082974241256,-0.14100387723139,
0.873638493505799));
#14122=CARTESIAN_POINT('Ctrl Pts',(0.0867012631995282,-0.127751761671338,
0.876285882880059));
#14123=CARTESIAN_POINT('Ctrl Pts',(0.12609672282758,-0.0890911788151255,
0.878933272254319));
#14124=CARTESIAN_POINT('Ctrl Pts',(0.140224208991091,-0.042730661487191,
0.88158066162858));
#14125=CARTESIAN_POINT('Ctrl Pts',(0.154351695154603,0.00362985584074295,
0.88422805100284));
#14126=CARTESIAN_POINT('Ctrl Pts',(0.143211207853577,0.057690307640398,
0.886875440377099));
#14127=CARTESIAN_POINT('Ctrl Pts',(0.111905662524754,0.09468823006692,0.889522829751359));
#14128=CARTESIAN_POINT('Ctrl Pts',(0.0806001171959318,0.131686152493442,
0.892170219125619));
#14129=CARTESIAN_POINT('Ctrl Pts',(0.0291295138393125,0.15162154554683,
0.894817608499879));
#14130=CARTESIAN_POINT('Ctrl Pts',(-0.0189299673197759,0.145362975188259,
0.897464997874139));
#14131=CARTESIAN_POINT('Ctrl Pts',(-0.0669894484788628,0.139104404829688,
0.9001123872484));
#14132=CARTESIAN_POINT('Ctrl Pts',(-0.11163780744042,0.10665187105916,0.902759776622659));
#14133=CARTESIAN_POINT('Ctrl Pts',(-0.132423802349956,0.0628703013313112,
0.905407165996919));
#14134=CARTESIAN_POINT('Ctrl Pts',(-0.141655418982822,0.043425734493323,
0.90658294246985));
#14135=CARTESIAN_POINT('Ctrl Pts',(-0.146180218154578,0.0217465313827003,
0.907758718942781));
#14136=CARTESIAN_POINT('Ctrl Pts',(-0.146121644853617,4.41067432152685E-5,
0.908934495415711));
#14137=CARTESIAN_POINT('Origin',(0.,0.,0.));
#14138=CARTESIAN_POINT('',(-0.146345621585321,-0.000133809880645736,0.966065504584291));
#14139=CARTESIAN_POINT('',(-0.146309694201085,-0.000133223314395004,0.958934495415711));
#14140=CARTESIAN_POINT('',(-0.14635,-1.79227059055215E-17,0.));
#14141=CARTESIAN_POINT('Ctrl Pts',(-0.146345621585321,-0.000133809880645736,
0.966065504584291));
#14142=CARTESIAN_POINT('Ctrl Pts',(-0.146004672532387,0.0370537288701324,
0.964042983538364));
#14143=CARTESIAN_POINT('Ctrl Pts',(-0.131578083002406,0.0744765756810296,
0.962020462492437));
#14144=CARTESIAN_POINT('Ctrl Pts',(-0.106003654037246,0.101251356830495,
0.959997941446511));
#14145=CARTESIAN_POINT('Ctrl Pts',(-0.0725412702228666,0.136284319036219,
0.957351611567409));
#14146=CARTESIAN_POINT('Ctrl Pts',(-0.0199938687303381,0.153087872523943,
0.954705281688306));
#14147=CARTESIAN_POINT('Ctrl Pts',(0.0275867780614433,0.143970766496025,
0.952058951809204));
#14148=CARTESIAN_POINT('Ctrl Pts',(0.0751674248532248,0.134853660468108,
0.949412621930102));
#14149=CARTESIAN_POINT('Ctrl Pts',(0.11778131694426,0.0998158949245492,
0.946766292051));
#14150=CARTESIAN_POINT('Ctrl Pts',(0.135923405490256,0.0548948063954655,
0.944119962171899));
#14151=CARTESIAN_POINT('Ctrl Pts',(0.154065494036253,0.0099737178663825,
0.941473632292797));
#14152=CARTESIAN_POINT('Ctrl Pts',(0.147735779037212,-0.0448306936482241,
0.938827302413695));
#14153=CARTESIAN_POINT('Ctrl Pts',(0.119831470632095,-0.0844335867733556,
0.936180972534593));
#14154=CARTESIAN_POINT('Ctrl Pts',(0.0919271622269763,-0.124036479898489,
0.933534642655491));
#14155=CARTESIAN_POINT('Ctrl Pts',(0.0424482604157787,-0.148437854634144,
0.93088831277639));
#14156=CARTESIAN_POINT('Ctrl Pts',(-0.00595796300272124,-0.146468817862788,
0.928241982897288));
#14157=CARTESIAN_POINT('Ctrl Pts',(-0.0543641864212212,-0.144499781091432,
0.925595653018186));
#14158=CARTESIAN_POINT('Ctrl Pts',(-0.101697731447024,-0.116160332813065,
0.922949323139084));
#14159=CARTESIAN_POINT('Ctrl Pts',(-0.126293289834417,-0.0744218843624929,
0.920302993259982));
#14160=CARTESIAN_POINT('Ctrl Pts',(-0.139421333187579,-0.052143709087005,
0.918890497034752));
#14161=CARTESIAN_POINT('Ctrl Pts',(-0.146071410932229,-0.0260482098028304,
0.917478000809521));
#14162=CARTESIAN_POINT('Ctrl Pts',(-0.146114231148477,2.69008449349656E-5,
0.916065504584291));
#14163=CARTESIAN_POINT('Ctrl Pts',(-0.146121644853617,4.41067432152685E-5,
0.908934495415711));
#14164=CARTESIAN_POINT('Ctrl Pts',(-0.146048333958771,-0.027118852224649,
0.910406108317041));
#14165=CARTESIAN_POINT('Ctrl Pts',(-0.138795050353101,-0.0543181883240968,
0.91187772121837));
#14166=CARTESIAN_POINT('Ctrl Pts',(-0.124603830013468,-0.0772180274565794,
0.9133493341197));
#14167=CARTESIAN_POINT('Ctrl Pts',(-0.0990742319099257,-0.118414180831446,
0.91599672349396));
#14168=CARTESIAN_POINT('Ctrl Pts',(-0.0510914048453256,-0.145695881896007,
0.91864411286822));
#14169=CARTESIAN_POINT('Ctrl Pts',(-0.00263394834681351,-0.146566710184873,
0.92129150224248));
#14170=CARTESIAN_POINT('Ctrl Pts',(0.0458235081516972,-0.147437538473739,
0.92393889161674));
#14171=CARTESIAN_POINT('Ctrl Pts',(0.0947555940841207,-0.121897493986912,
0.926586280990999));
#14172=CARTESIAN_POINT('Ctrl Pts',(0.121748900601314,-0.0816452290135895,
0.929233670365259));
#14173=CARTESIAN_POINT('Ctrl Pts',(0.148742207118509,-0.0413929640402651,
0.931881059739519));
#14174=CARTESIAN_POINT('Ctrl Pts',(0.153796734220472,0.0135715214195569,
0.93452844911378));
#14175=CARTESIAN_POINT('Ctrl Pts',(0.134597248858856,0.0580716696672091,
0.93717583848804));
#14176=CARTESIAN_POINT('Ctrl Pts',(0.115397763497239,0.102571817914861,
0.9398232278623));
#14177=CARTESIAN_POINT('Ctrl Pts',(0.0719442656720451,0.136607628950342,
0.942470617236559));
#14178=CARTESIAN_POINT('Ctrl Pts',(0.0241406894609324,0.144588953003544,
0.945118006610819));
#14179=CARTESIAN_POINT('Ctrl Pts',(-0.023662886750181,0.152570277056746,
0.947765395985079));
#14180=CARTESIAN_POINT('Ctrl Pts',(-0.0758165413472122,0.134497114127667,
0.950412785359339));
#14181=CARTESIAN_POINT('Ctrl Pts',(-0.108431221550465,0.0986479012011113,
0.953060174733599));
#14182=CARTESIAN_POINT('Ctrl Pts',(-0.132554242808212,0.0721325001574252,
0.955018281627637));
#14183=CARTESIAN_POINT('Ctrl Pts',(-0.145988218858404,0.0358924841874147,
0.956976388521674));
#14184=CARTESIAN_POINT('Ctrl Pts',(-0.146309694201085,-0.000133223314395004,
0.958934495415711));
#14185=CARTESIAN_POINT('Origin',(0.,0.,0.));
#14186=CARTESIAN_POINT('',(-0.146565171121453,5.44893591410845E-5,1.01606550458429));
#14187=CARTESIAN_POINT('',(-0.146582076026177,3.15354312248815E-5,1.00893449541571));
#14188=CARTESIAN_POINT('',(-0.14635,-1.79227059055215E-17,0.));
#14189=CARTESIAN_POINT('Ctrl Pts',(-0.146565171121453,5.44893591410845E-5,
1.01606550458429));
#14190=CARTESIAN_POINT('Ctrl Pts',(-0.146579596851449,0.00307427920823236,
1.01590062602541));
#14191=CARTESIAN_POINT('Ctrl Pts',(-0.146494352296349,0.00609323927190738,
1.01573574746653));
#14192=CARTESIAN_POINT('Ctrl Pts',(-0.146306854564556,0.00910583530985269,
1.01557086890765));
#14193=CARTESIAN_POINT('Ctrl Pts',(-0.143297482980539,0.0574585317612167,
1.01292453902855));
#14194=CARTESIAN_POINT('Ctrl Pts',(-0.11394685994478,0.104171803331984,
1.01027820914945));
#14195=CARTESIAN_POINT('Ctrl Pts',(-0.0716892273871119,0.127864250695428,
1.00763187927034));
#14196=CARTESIAN_POINT('Ctrl Pts',(-0.0294315948294418,0.151556698058874,
1.00498554939124));
#14197=CARTESIAN_POINT('Ctrl Pts',(0.0257330472501378,0.152228321214993,
1.00233921951214));
#14198=CARTESIAN_POINT('Ctrl Pts',(0.0685549742796134,0.129571707678744,
0.999692889633039));
#14199=CARTESIAN_POINT('Ctrl Pts',(0.111376901309088,0.106915094142495,
0.997046559753937));
#14200=CARTESIAN_POINT('Ctrl Pts',(0.141856113288459,0.0609302439138786,
0.994400229874835));
#14201=CARTESIAN_POINT('Ctrl Pts',(0.146041795372579,0.0126651464112397,
0.991753899995733));
#14202=CARTESIAN_POINT('Ctrl Pts',(0.150227477456699,-0.0355999510913994,
0.989107570116631));
#14203=CARTESIAN_POINT('Ctrl Pts',(0.128119629645567,-0.0861452958680607,
0.986461240237529));
#14204=CARTESIAN_POINT('Ctrl Pts',(0.0898373616998479,-0.115835488396583,
0.983814910358427));
#14205=CARTESIAN_POINT('Ctrl Pts',(0.051555093754129,-0.145525680925106,
0.981168580479325));
#14206=CARTESIAN_POINT('Ctrl Pts',(-0.00290159432617693,-0.154360721205491,
0.978522250600224));
#14207=CARTESIAN_POINT('Ctrl Pts',(-0.0486070196525971,-0.138296672301818,
0.975875920721122));
#14208=CARTESIAN_POINT('Ctrl Pts',(-0.0943124449790173,-0.122232623398145,
0.97322959084202));
#14209=CARTESIAN_POINT('Ctrl Pts',(-0.131266607551552,-0.081269485310415,
0.970583260962917));
#14210=CARTESIAN_POINT('Ctrl Pts',(-0.142555005769704,-0.0341567308046872,
0.967936931083816));
#14211=CARTESIAN_POINT('Ctrl Pts',(-0.145215975052668,-0.0230510282813687,
0.967313122250641));
#14212=CARTESIAN_POINT('Ctrl Pts',(-0.146450780951306,-0.0116036114945705,
0.966689313417466));
#14213=CARTESIAN_POINT('Ctrl Pts',(-0.146345621585321,-0.000133809880645736,
0.966065504584291));
#14214=CARTESIAN_POINT('Ctrl Pts',(-0.146309694201085,-0.000133223314395004,
0.958934495415711));
#14215=CARTESIAN_POINT('Ctrl Pts',(-0.146422858258782,-0.0128148032088542,
0.959623777895933));
#14216=CARTESIAN_POINT('Ctrl Pts',(-0.14491119500038,-0.0254698272036438,
0.960313060376156));
#14217=CARTESIAN_POINT('Ctrl Pts',(-0.141668994059001,-0.037664762585484,
0.961002342856379));
#14218=CARTESIAN_POINT('Ctrl Pts',(-0.129216380554811,-0.0845029505214961,
0.963649732230639));
#14219=CARTESIAN_POINT('Ctrl Pts',(-0.0912354477369537,-0.12455406346949,
0.966297121604899));
#14220=CARTESIAN_POINT('Ctrl Pts',(-0.0451234138007503,-0.1394726343957,
0.968944510979159));
#14221=CARTESIAN_POINT('Ctrl Pts',(0.00098862013545236,-0.154391205321909,
0.97159190035342));
#14222=CARTESIAN_POINT('Ctrl Pts',(0.055231755190001,-0.144177234226336,
0.974239289727679));
#14223=CARTESIAN_POINT('Ctrl Pts',(0.0927598492034174,-0.113509244531313,
0.976886679101939));
#14224=CARTESIAN_POINT('Ctrl Pts',(0.130287943216833,-0.0828412548362905,
0.979534068476199));
#14225=CARTESIAN_POINT('Ctrl Pts',(0.151100996189117,-0.0317192465418168,
0.982181457850459));
#14226=CARTESIAN_POINT('Ctrl Pts',(0.145665560755875,0.0164402745715088,
0.984828847224719));
#14227=CARTESIAN_POINT('Ctrl Pts',(0.140230125322634,0.0645997956848379,
0.987476236598979));
#14228=CARTESIAN_POINT('Ctrl Pts',(0.108546201483865,0.109796829617019,
0.990123625973239));
#14229=CARTESIAN_POINT('Ctrl Pts',(0.0651266538643092,0.131328813193254,
0.992771015347499));
#14230=CARTESIAN_POINT('Ctrl Pts',(0.0217071062447581,0.152860796769488,
0.995418404721759));
#14231=CARTESIAN_POINT('Ctrl Pts',(-0.0334480651555777,0.15072772998978,
0.998065794096019));
#14232=CARTESIAN_POINT('Ctrl Pts',(-0.0750749586823209,0.125906667008376,
1.00071318347028));
#14233=CARTESIAN_POINT('Ctrl Pts',(-0.116701852209067,0.101085604026969,
1.00336057284454));
#14234=CARTESIAN_POINT('Ctrl Pts',(-0.144800467862219,0.053576544843864,
1.0060079622188));
#14235=CARTESIAN_POINT('Ctrl Pts',(-0.146500196332402,0.00514107896046776,
1.00865535159306));
#14236=CARTESIAN_POINT('Ctrl Pts',(-0.146559936783033,0.00343871495990628,
1.00874839953394));
#14237=CARTESIAN_POINT('Ctrl Pts',(-0.146587066279139,0.00173520655478852,
1.00884144747483));
#14238=CARTESIAN_POINT('Ctrl Pts',(-0.146582076026177,3.15354312248815E-5,
1.00893449541571));
#14239=CARTESIAN_POINT('Origin',(0.,0.,0.));
#14240=CARTESIAN_POINT('',(-0.146184049129756,9.96948043307314E-5,1.06606550458429));
#14241=CARTESIAN_POINT('',(-0.146216477546812,0.000114345603752017,1.05893449541571));
#14242=CARTESIAN_POINT('',(-0.14635,-1.79227059055215E-17,0.));
#14243=CARTESIAN_POINT('Ctrl Pts',(-0.146184049129756,9.96948043307314E-5,
1.06606550458429));
#14244=CARTESIAN_POINT('Ctrl Pts',(-0.146294264763128,0.0176817746259609,
1.06511193863336));
#14245=CARTESIAN_POINT('Ctrl Pts',(-0.143360807533043,0.0352283113603788,
1.06415837268242));
#14246=CARTESIAN_POINT('Ctrl Pts',(-0.13721959397524,0.0515693218739058,
1.06320480673148));
#14247=CARTESIAN_POINT('Ctrl Pts',(-0.120176538991979,0.0969187854681546,
1.06055847685238));
#14248=CARTESIAN_POINT('Ctrl Pts',(-0.0784283132238915,0.132983650068601,
1.05791214697328));
#14249=CARTESIAN_POINT('Ctrl Pts',(-0.0310837364199337,0.143256459747686,
1.05526581709418));
#14250=CARTESIAN_POINT('Ctrl Pts',(0.0162608403840241,0.153529269426771,
1.05261948721508));
#14251=CARTESIAN_POINT('Ctrl Pts',(0.0692017682238519,0.138010024184496,
1.04997315733597));
#14252=CARTESIAN_POINT('Ctrl Pts',(0.103507151520239,0.103802126728842,
1.04732682745687));
#14253=CARTESIAN_POINT('Ctrl Pts',(0.137812534816628,0.0695942292731864,
1.04468049757777));
#14254=CARTESIAN_POINT('Ctrl Pts',(0.153482373569574,0.01669767960415,1.04203416769867));
#14255=CARTESIAN_POINT('Ctrl Pts',(0.143344336052008,-0.0306759392859165,
1.03938783781957));
#14256=CARTESIAN_POINT('Ctrl Pts',(0.133206298534443,-0.0780495581759789,
1.03674150794047));
#14257=CARTESIAN_POINT('Ctrl Pts',(0.0972603847463712,-0.119900246287072,
1.03409517806136));
#14258=CARTESIAN_POINT('Ctrl Pts',(0.0519596049571008,-0.137072285243832,
1.03144884818226));
#14259=CARTESIAN_POINT('Ctrl Pts',(0.00665882516783032,-0.154244324200591,
1.02880251830316));
#14260=CARTESIAN_POINT('Ctrl Pts',(-0.0479968206226384,-0.146737714003016,
1.02615618842406));
#14261=CARTESIAN_POINT('Ctrl Pts',(-0.0869905834517384,-0.11798834823825,
1.02350985854496));
#14262=CARTESIAN_POINT('Ctrl Pts',(-0.123554854979944,-0.0910302005802824,
1.02102840722473));
#14263=CARTESIAN_POINT('Ctrl Pts',(-0.146348061346918,-0.0453938791777224,
1.01854695590451));
#14264=CARTESIAN_POINT('Ctrl Pts',(-0.146565171121453,5.44893591410845E-5,
1.01606550458429));
#14265=CARTESIAN_POINT('Ctrl Pts',(-0.146582076026177,3.15354312248815E-5,
1.00893449541571));
#14266=CARTESIAN_POINT('Ctrl Pts',(-0.146445084172466,-0.0467374494427972,
1.01148883684909));
#14267=CARTESIAN_POINT('Ctrl Pts',(-0.122102455869861,-0.0936290599181376,
1.01404317828246));
#14268=CARTESIAN_POINT('Ctrl Pts',(-0.0837162036049941,-0.120334265578335,
1.01659751971584));
#14269=CARTESIAN_POINT('Ctrl Pts',(-0.0439316411201867,-0.14801227165006,
1.0192449090901));
#14270=CARTESIAN_POINT('Ctrl Pts',(0.0109383251366414,-0.154006411209824,
1.02189229846436));
#14271=CARTESIAN_POINT('Ctrl Pts',(0.0557604321169594,-0.135571060438576,
1.02453968783862));
#14272=CARTESIAN_POINT('Ctrl Pts',(0.100582539097277,-0.11713570966733,
1.02718707721288));
#14273=CARTESIAN_POINT('Ctrl Pts',(0.135356786801084,-0.0742708685650716,
1.02983446658714));
#14274=CARTESIAN_POINT('Ctrl Pts',(0.144154783532934,-0.0266108361928598,
1.0324818559614));
#14275=CARTESIAN_POINT('Ctrl Pts',(0.152952780264784,0.0210491961793507,
1.03512924533566));
#14276=CARTESIAN_POINT('Ctrl Pts',(0.135774526024679,0.0735044198215165,
1.03777663470992));
#14277=CARTESIAN_POINT('Ctrl Pts',(0.100488543649143,0.106727647840587,
1.04042402408418));
#14278=CARTESIAN_POINT('Ctrl Pts',(0.0652025612736062,0.139950875859659,
1.04307141345844));
#14279=CARTESIAN_POINT('Ctrl Pts',(0.0118088507626404,0.153942108255635,
1.0457188028327));
#14280=CARTESIAN_POINT('Ctrl Pts',(-0.0352355257975899,0.142292641904202,
1.04836619220696));
#14281=CARTESIAN_POINT('Ctrl Pts',(-0.0822799023578202,0.130643175552769,
1.05101358158122));
#14282=CARTESIAN_POINT('Ctrl Pts',(-0.122974944967313,0.0933530104539243,
1.05366097095548));
#14283=CARTESIAN_POINT('Ctrl Pts',(-0.138680233730631,0.0475029577050484,
1.05630836032974));
#14284=CARTESIAN_POINT('Ctrl Pts',(-0.143873300563147,0.0323423075707214,
1.05718373869173));
#14285=CARTESIAN_POINT('Ctrl Pts',(-0.146334133026589,0.0162457690968458,
1.05805911705372));
#14286=CARTESIAN_POINT('Ctrl Pts',(-0.146216477546812,0.000114345603752017,
1.05893449541571));
#14287=CARTESIAN_POINT('Origin',(0.,0.,0.));
#14288=CARTESIAN_POINT('',(-0.146204073634541,-0.000109175101205505,1.11606550458429));
#14289=CARTESIAN_POINT('',(-0.146170555016798,-9.22629125885076E-5,1.10893449541571));
#14290=CARTESIAN_POINT('',(-0.14635,-1.79227059055215E-17,0.));
#14291=CARTESIAN_POINT('Ctrl Pts',(-0.146204073634541,-0.000109175101205505,
1.11606550458429));
#14292=CARTESIAN_POINT('Ctrl Pts',(-0.145981599624502,0.032003853555373,
1.1143232512413));
#14293=CARTESIAN_POINT('Ctrl Pts',(-0.135565881201595,0.0642480963468658,
1.11258099789831));
#14294=CARTESIAN_POINT('Ctrl Pts',(-0.11609067353381,0.0895073597405865,
1.11083874455532));
#14295=CARTESIAN_POINT('Ctrl Pts',(-0.0865095427755784,0.127873963375947,
1.10819241467622));
#14296=CARTESIAN_POINT('Ctrl Pts',(-0.0360273159486943,0.150125560802435,
1.10554608479712));
#14297=CARTESIAN_POINT('Ctrl Pts',(0.0122494975033169,0.14607724579886,
1.10289975491801));
#14298=CARTESIAN_POINT('Ctrl Pts',(0.0605263109553308,0.142028930795284,
1.10025342503891));
#14299=CARTESIAN_POINT('Ctrl Pts',(0.10659771103247,0.111680703361642,1.09760709515981));
#14300=CARTESIAN_POINT('Ctrl Pts',(0.129376093089052,0.0689234246557527,
1.09496076528071));
#14301=CARTESIAN_POINT('Ctrl Pts',(0.152154475145634,0.0261661459498645,
1.09231443540161));
#14302=CARTESIAN_POINT('Ctrl Pts',(0.151639839181659,-0.0290001840282729,
1.0896681055225));
#14303=CARTESIAN_POINT('Ctrl Pts',(0.128067742174483,-0.0713250681289163,
1.0870217756434));
#14304=CARTESIAN_POINT('Ctrl Pts',(0.104495645167307,-0.11364995222956,
1.0843754457643));
#14305=CARTESIAN_POINT('Ctrl Pts',(0.0578660871169326,-0.143133390452712,
1.0817291158852));
#14306=CARTESIAN_POINT('Ctrl Pts',(0.00952215035475689,-0.146280349267719,
1.0790827860061));
#14307=CARTESIAN_POINT('Ctrl Pts',(-0.0388217864074202,-0.149427308082725,
1.07643645612699));
#14308=CARTESIAN_POINT('Ctrl Pts',(-0.0888801018813974,-0.126237787489585,
1.07379012624789));
#14309=CARTESIAN_POINT('Ctrl Pts',(-0.117740317519168,-0.0873259958989869,
1.07114379636879));
#14310=CARTESIAN_POINT('Ctrl Pts',(-0.136201180005177,-0.0624354946409797,
1.06945103244062));
#14311=CARTESIAN_POINT('Ctrl Pts',(-0.145988395071105,-0.0311118962502767,
1.06775826851246));
#14312=CARTESIAN_POINT('Ctrl Pts',(-0.146184049129756,9.96948043307314E-5,
1.06606550458429));
#14313=CARTESIAN_POINT('Ctrl Pts',(-0.146216477546812,0.000114345603752017,
1.05893449541571));
#14314=CARTESIAN_POINT('Ctrl Pts',(-0.145978309898544,-0.0325401742182177,
1.06070650642798));
#14315=CARTESIAN_POINT('Ctrl Pts',(-0.135174246449945,-0.06533764273189,
1.06247851744025));
#14316=CARTESIAN_POINT('Ctrl Pts',(-0.115079600404687,-0.0908043159161929,
1.06425052845252));
#14317=CARTESIAN_POINT('Ctrl Pts',(-0.0850581433982766,-0.128851596389654,
1.06689791782678));
#14318=CARTESIAN_POINT('Ctrl Pts',(-0.0342996944683099,-0.150536216937668,
1.06954530720104));
#14319=CARTESIAN_POINT('Ctrl Pts',(0.0139457694684962,-0.145925507476389,
1.0721926965753));
#14320=CARTESIAN_POINT('Ctrl Pts',(0.0621912334052997,-0.14131479801511,
1.07484008594956));
#14321=CARTESIAN_POINT('Ctrl Pts',(0.107923712348941,-0.110408758544542,
1.07748747532382));
#14322=CARTESIAN_POINT('Ctrl Pts',(0.1301953818052,-0.0673639426912374,
1.08013486469808));
#14323=CARTESIAN_POINT('Ctrl Pts',(0.15246705126146,-0.024319126837932,
1.08278225407234));
#14324=CARTESIAN_POINT('Ctrl Pts',(0.151277911230334,0.0308644653981125,
1.0854296434466));
#14325=CARTESIAN_POINT('Ctrl Pts',(0.127172648928576,0.0729099141598672,
1.08807703282086));
#14326=CARTESIAN_POINT('Ctrl Pts',(0.103067386626818,0.114955362921624,
1.09072442219512));
#14327=CARTESIAN_POINT('Ctrl Pts',(0.0560460020544268,0.143862668209093,
1.09337181156938));
#14328=CARTESIAN_POINT('Ctrl Pts',(0.00764670469074742,0.146390799320458,
1.09601920094364));
#14329=CARTESIAN_POINT('Ctrl Pts',(-0.0407525926729279,0.148918930431823,
1.0986665903179));
#14330=CARTESIAN_POINT('Ctrl Pts',(-0.0905298028278899,0.125067887367091,
1.10131397969216));
#14331=CARTESIAN_POINT('Ctrl Pts',(-0.11888440661962,0.0857626730052823,
1.10396136906642));
#14332=CARTESIAN_POINT('Ctrl Pts',(-0.136639133674055,0.0611510311732957,
1.10561907784952));
#14333=CARTESIAN_POINT('Ctrl Pts',(-0.145994366384503,0.0304800321277272,
1.10727678663261));
#14334=CARTESIAN_POINT('Ctrl Pts',(-0.146170555016798,-9.22629125885076E-5,
1.10893449541571));
#14335=CARTESIAN_POINT('Origin',(0.,0.,0.));
#14336=CARTESIAN_POINT('',(-0.146577386142569,-3.88073511912723E-5,1.16606550458429));
#14337=CARTESIAN_POINT('',(-0.146552328192774,-6.73160170860698E-5,1.15893449541571));
#14338=CARTESIAN_POINT('',(-0.14635,-1.79227059055215E-17,0.));
#14339=CARTESIAN_POINT('Ctrl Pts',(-0.146577386142569,-3.88073511912723E-5,
1.16606550458429));
#14340=CARTESIAN_POINT('Ctrl Pts',(-0.146413350709018,0.0463056768050285,
1.16353456384924));
#14341=CARTESIAN_POINT('Ctrl Pts',(-0.122574225104448,0.0927954474992645,
1.1610036231142));
#14342=CARTESIAN_POINT('Ctrl Pts',(-0.0847742546295189,0.119590709008994,
1.15847268237915));
#14343=CARTESIAN_POINT('Ctrl Pts',(-0.0452509303920754,0.147607604138013,
1.15582635250005));
#14344=CARTESIAN_POINT('Ctrl Pts',(0.00953524646069181,0.154093252855687,
1.15318002262095));
#14345=CARTESIAN_POINT('Ctrl Pts',(0.0545077808453859,0.136079071706768,
1.15053369274185));
#14346=CARTESIAN_POINT('Ctrl Pts',(0.0994803152300801,0.118064890557849,
1.14788736286275));
#14347=CARTESIAN_POINT('Ctrl Pts',(0.134639207146701,0.0755508795423365,
1.14524103298364));
#14348=CARTESIAN_POINT('Ctrl Pts',(0.14389167861853,0.027996370364851,1.14259470310454));
#14349=CARTESIAN_POINT('Ctrl Pts',(0.15314415009036,-0.0195581388126345,
1.13994837322544));
#14350=CARTESIAN_POINT('Ctrl Pts',(0.136490201117397,-0.0721531461520931,
1.13730204334634));
#14351=CARTESIAN_POINT('Ctrl Pts',(0.101552606157185,-0.105715089329518,
1.13465571346724));
#14352=CARTESIAN_POINT('Ctrl Pts',(0.0666150111969725,-0.139277032506943,
1.13200938358813));
#14353=CARTESIAN_POINT('Ctrl Pts',(0.0133937702495101,-0.153805911522335,
1.12936305370903));
#14354=CARTESIAN_POINT('Ctrl Pts',(-0.033750917386428,-0.142651629870951,
1.12671672382993));
#14355=CARTESIAN_POINT('Ctrl Pts',(-0.0808956050223675,-0.131497348219567,
1.12407039395083));
#14356=CARTESIAN_POINT('Ctrl Pts',(-0.121963739346782,-0.094659905901407,
1.12142406407173));
#14357=CARTESIAN_POINT('Ctrl Pts',(-0.1381577891642,-0.0490003798202082,
1.11877773419262));
#14358=CARTESIAN_POINT('Ctrl Pts',(-0.143690228857438,-0.0334015285560649,
1.11787365765651));
#14359=CARTESIAN_POINT('Ctrl Pts',(-0.146319518115206,-0.0167730178360648,
1.1169695811204));
#14360=CARTESIAN_POINT('Ctrl Pts',(-0.146204073634541,-0.000109175101205505,
1.11606550458429));
#14361=CARTESIAN_POINT('Ctrl Pts',(-0.146170555016798,-9.22629125885076E-5,
1.10893449541571));
#14362=CARTESIAN_POINT('Ctrl Pts',(-0.146275742653821,-0.0183444476975235,
1.10992417600687));
#14363=CARTESIAN_POINT('Ctrl Pts',(-0.143109248288425,-0.0365614514641733,
1.11091385659804));
#14364=CARTESIAN_POINT('Ctrl Pts',(-0.136505188007283,-0.0534328725168923,
1.1119035371892));
#14365=CARTESIAN_POINT('Ctrl Pts',(-0.118839368174718,-0.0985638180183679,
1.11455092656346));
#14366=CARTESIAN_POINT('Ctrl Pts',(-0.0765757310810901,-0.134066323362434,
1.11719831593772));
#14367=CARTESIAN_POINT('Ctrl Pts',(-0.0290731934694857,-0.143678417446031,
1.11984570531198));
#14368=CARTESIAN_POINT('Ctrl Pts',(0.01842934414212,-0.153290511529629,
1.12249309468624));
#14369=CARTESIAN_POINT('Ctrl Pts',(0.071170782271703,-0.137012194352758,
1.1251404840605));
#14370=CARTESIAN_POINT('Ctrl Pts',(0.10499283308901,-0.102299771349957,
1.12778787343476));
#14371=CARTESIAN_POINT('Ctrl Pts',(0.138814883906317,-0.0675873483471558,
1.13043526280902));
#14372=CARTESIAN_POINT('Ctrl Pts',(0.153717547411349,-0.0144408195184256,
1.13308265218328));
#14373=CARTESIAN_POINT('Ctrl Pts',(0.142874638214406,0.0327959749574983,
1.13573004155754));
#14374=CARTESIAN_POINT('Ctrl Pts',(0.132031729017462,0.0800327694334235,
1.1383774309318));
#14375=CARTESIAN_POINT('Ctrl Pts',(0.0954432471185425,0.121359829556542,
1.14102482030606));
#14376=CARTESIAN_POINT('Ctrl Pts',(0.0498685966661331,0.137847238945365,
1.14367220968032));
#14377=CARTESIAN_POINT('Ctrl Pts',(0.00429394621372511,0.154334648334189,
1.14631959905458));
#14378=CARTESIAN_POINT('Ctrl Pts',(-0.0502668727921719,0.145982406988718,
1.14896698842884));
#14379=CARTESIAN_POINT('Ctrl Pts',(-0.0888222026239048,0.116616270474356,
1.1516143778031));
#14380=CARTESIAN_POINT('Ctrl Pts',(-0.124357782404925,0.0895501633622979,
1.1540544170073));
#14381=CARTESIAN_POINT('Ctrl Pts',(-0.146296868742479,0.0446329749882746,
1.15649445621151));
#14382=CARTESIAN_POINT('Ctrl Pts',(-0.146552328192774,-6.73160170860698E-5,
1.15893449541571));
#14383=CARTESIAN_POINT('Origin',(0.,0.,0.));
#14384=CARTESIAN_POINT('',(-0.146318311025392,0.000133437649768732,1.21606550458429));
#14385=CARTESIAN_POINT('',(-0.146373054956946,0.000132657382717961,1.20893449541571));
#14386=CARTESIAN_POINT('',(-0.14635,-1.79227059055215E-17,0.));
#14387=CARTESIAN_POINT('Ctrl Pts',(-0.146318311025392,0.000133437649768732,
1.21606550458429));
#14388=CARTESIAN_POINT('Ctrl Pts',(-0.146429658069886,0.0125190846592594,
1.21539220633629));
#14389=CARTESIAN_POINT('Ctrl Pts',(-0.144988168643405,0.0248791929292086,
1.21471890808829));
#14390=CARTESIAN_POINT('Ctrl Pts',(-0.141892968227885,0.0368102906365087,
1.21404560984029));
#14391=CARTESIAN_POINT('Ctrl Pts',(-0.129727599662405,0.083704249513052,
1.21139927996119));
#14392=CARTESIAN_POINT('Ctrl Pts',(-0.0920156607298113,0.123970842060419,
1.20875295008209));
#14393=CARTESIAN_POINT('Ctrl Pts',(-0.0460184991925076,0.139179415364965,
1.20610662020299));
#14394=CARTESIAN_POINT('Ctrl Pts',(-2.13376552038805E-5,0.15438798866951,
1.20346029032389));
#14395=CARTESIAN_POINT('Ctrl Pts',(0.0542610464868107,0.144538542731236,
1.20081396044478));
#14396=CARTESIAN_POINT('Ctrl Pts',(0.091982751999895,0.114139323915075,
1.19816763056568));
#14397=CARTESIAN_POINT('Ctrl Pts',(0.129704457512977,0.0837401050989159,
1.19552130068658));
#14398=CARTESIAN_POINT('Ctrl Pts',(0.150865484397133,0.0327911134048729,
1.19287497080748));
#14399=CARTESIAN_POINT('Ctrl Pts',(0.145780097726084,-0.0153874961003253,
1.19022864092838));
#14400=CARTESIAN_POINT('Ctrl Pts',(0.140694711055036,-0.063566105605525,
1.18758231104927));
#14401=CARTESIAN_POINT('Ctrl Pts',(0.109362910828785,-0.108974332921877,
1.18493598117017));
#14402=CARTESIAN_POINT('Ctrl Pts',(0.0661257549466402,-0.130828118009858,
1.18228965129107));
#14403=CARTESIAN_POINT('Ctrl Pts',(0.0228885990644955,-0.152681903097838,
1.17964332141197));
#14404=CARTESIAN_POINT('Ctrl Pts',(-0.0322539124735426,-0.150981245957443,
1.17699699153287));
#14405=CARTESIAN_POINT('Ctrl Pts',(-0.0740621845924981,-0.126504564117865,
1.17435066165376));
#14406=CARTESIAN_POINT('Ctrl Pts',(-0.115870456711455,-0.102027882278287,
1.17170433177466));
#14407=CARTESIAN_POINT('Ctrl Pts',(-0.144344489411329,-0.0547751757395235,
1.16905800189556));
#14408=CARTESIAN_POINT('Ctrl Pts',(-0.146451269950206,-0.00637475169995868,
1.16641167201646));
#14409=CARTESIAN_POINT('Ctrl Pts',(-0.146543132875163,-0.00426432565444621,
1.1662962828724));
#14410=CARTESIAN_POINT('Ctrl Pts',(-0.146584864748453,-0.00215171749738942,
1.16618089372835));
#14411=CARTESIAN_POINT('Ctrl Pts',(-0.146577386142569,-3.88073511912723E-5,
1.16606550458429));
#14412=CARTESIAN_POINT('Ctrl Pts',(-0.146552328192774,-6.73160170860698E-5,
1.15893449541571));
#14413=CARTESIAN_POINT('Ctrl Pts',(-0.146574036680232,-0.00386586684592084,
1.15914184558577));
#14414=CARTESIAN_POINT('Ctrl Pts',(-0.1464391612665,-0.00766285139452399,
1.15934919575582));
#14415=CARTESIAN_POINT('Ctrl Pts',(-0.146142739258869,-0.0114471821958193,
1.15955654592588));
#14416=CARTESIAN_POINT('Ctrl Pts',(-0.142358105404532,-0.0597644666683822,
1.16220393530014));
#14417=CARTESIAN_POINT('Ctrl Pts',(-0.112238997038288,-0.106019003930254,
1.1648513246744));
#14418=CARTESIAN_POINT('Ctrl Pts',(-0.0695815129186611,-0.129023839960917,
1.16749871404866));
#14419=CARTESIAN_POINT('Ctrl Pts',(-0.026924028799035,-0.15202867599158,
1.17014610342292));
#14420=CARTESIAN_POINT('Ctrl Pts',(0.0282718310739737,-0.151783810791035,
1.17279349279718));
#14421=CARTESIAN_POINT('Ctrl Pts',(0.0707235276354612,-0.128401405199111,
1.17544088217144));
#14422=CARTESIAN_POINT('Ctrl Pts',(0.11317522419695,-0.105018999607187,
1.1780882715457));
#14423=CARTESIAN_POINT('Ctrl Pts',(0.142882757446916,-0.0584990536238821,
1.18073566091996));
#14424=CARTESIAN_POINT('Ctrl Pts',(0.146238551171451,-0.0101500920973681,
1.18338305029422));
#14425=CARTESIAN_POINT('Ctrl Pts',(0.149594344895986,0.0381988694291446,
1.18603043966848));
#14426=CARTESIAN_POINT('Ctrl Pts',(0.12659839909509,0.0883768464988665,
1.18867782904274));
#14427=CARTESIAN_POINT('Ctrl Pts',(0.0877840381772113,0.117399748124142,
1.191325218417));
#14428=CARTESIAN_POINT('Ctrl Pts',(0.0489696772593311,0.146422649749419,
1.19397260779126));
#14429=CARTESIAN_POINT('Ctrl Pts',(-0.00566309877553352,0.154290475930249,
1.19661999716552));
#14430=CARTESIAN_POINT('Ctrl Pts',(-0.0510896721842483,0.137399358129564,
1.19926738653978));
#14431=CARTESIAN_POINT('Ctrl Pts',(-0.0965162455929618,0.12050824032888,
1.20191477591404));
#14432=CARTESIAN_POINT('Ctrl Pts',(-0.132736616375526,0.0788581785466829,
1.2045621652883));
#14433=CARTESIAN_POINT('Ctrl Pts',(-0.143159994183491,0.0315270405159292,
1.20720955466256));
#14434=CARTESIAN_POINT('Ctrl Pts',(-0.145423823013163,0.021247302336111,
1.20778453491361));
#14435=CARTESIAN_POINT('Ctrl Pts',(-0.146470795531708,0.0106995851133921,
1.20835951516466));
#14436=CARTESIAN_POINT('Ctrl Pts',(-0.146373054956946,0.000132657382717961,
1.20893449541571));
#14437=CARTESIAN_POINT('Origin',(0.,0.,0.));
#14438=CARTESIAN_POINT('',(-0.146120596765396,-4.14129048147555E-5,1.26606550458429));
#14439=CARTESIAN_POINT('',(-0.146109918970638,-1.0198006988139E-5,1.25893449541571));
#14440=CARTESIAN_POINT('',(-0.14635,-1.79227059055215E-17,0.));
#14441=CARTESIAN_POINT('Ctrl Pts',(-0.146120596765396,-4.14129048147555E-5,
1.26606550458429));
#14442=CARTESIAN_POINT('Ctrl Pts',(-0.14605219935785,0.0269443530192317,
1.26460351894424));
#14443=CARTESIAN_POINT('Ctrl Pts',(-0.138898723445843,0.053963836666407,
1.26314153330418));
#14444=CARTESIAN_POINT('Ctrl Pts',(-0.124882896249422,0.0767650581554474,
1.26167954766413));
#14445=CARTESIAN_POINT('Ctrl Pts',(-0.0995129464537159,0.118037388097231,
1.25903321778503));
#14446=CARTESIAN_POINT('Ctrl Pts',(-0.051658938874944,0.145488850208621,
1.25638688790592));
#14447=CARTESIAN_POINT('Ctrl Pts',(-0.00322440565727106,0.146554478394238,
1.25374055802682));
#14448=CARTESIAN_POINT('Ctrl Pts',(0.0452101275604033,0.147620106579856,
1.25109422814772));
#14449=CARTESIAN_POINT('Ctrl Pts',(0.0942251864169787,0.122299900839699,
1.24844789826862));
#14450=CARTESIAN_POINT('Ctrl Pts',(0.121385807331354,0.0821833176976391,
1.24580156838952));
#14451=CARTESIAN_POINT('Ctrl Pts',(0.148546428245729,0.0420667345555804,
1.24315523851041));
#14452=CARTESIAN_POINT('Ctrl Pts',(0.153852611217905,-0.0128462259883804,
1.24050890863131));
#14453=CARTESIAN_POINT('Ctrl Pts',(0.134875632820701,-0.0574210379606392,
1.23786257875221));
#14454=CARTESIAN_POINT('Ctrl Pts',(0.115898654423498,-0.101995849932898,
1.23521624887311));
#14455=CARTESIAN_POINT('Ctrl Pts',(0.0726385146569148,-0.136232513333455,
1.23256991899401));
#14456=CARTESIAN_POINT('Ctrl Pts',(0.0248960600935515,-0.144460368686643,
1.2299235891149));
#14457=CARTESIAN_POINT('Ctrl Pts',(-0.0228463944698117,-0.152688224039831,
1.2272772592358));
#14458=CARTESIAN_POINT('Ctrl Pts',(-0.0750711638299551,-0.134907271345651,
1.2246309293567));
#14459=CARTESIAN_POINT('Ctrl Pts',(-0.107874149410843,-0.0992561323957017,
1.2219845994776));
#14460=CARTESIAN_POINT('Ctrl Pts',(-0.132331163880887,-0.072675612185966,
1.2200115678465));
#14461=CARTESIAN_POINT('Ctrl Pts',(-0.145992019903337,-0.0361614337449312,
1.21803853621539));
#14462=CARTESIAN_POINT('Ctrl Pts',(-0.146318311025392,0.000133437649768732,
1.21606550458429));
#14463=CARTESIAN_POINT('Ctrl Pts',(-0.146373054956946,0.000132657382717961,
1.20893449541571));
#14464=CARTESIAN_POINT('Ctrl Pts',(-0.146020767276673,-0.0379538636644633,
1.21100690453892));
#14465=CARTESIAN_POINT('Ctrl Pts',(-0.130797424420382,-0.0762899498869128,
1.21307931366213));
#14466=CARTESIAN_POINT('Ctrl Pts',(-0.104081054125652,-0.103227285106232,
1.21515172278534));
#14467=CARTESIAN_POINT('Ctrl Pts',(-0.0699523514264828,-0.137638258418326,
1.2177991121596));
#14468=CARTESIAN_POINT('Ctrl Pts',(-0.0170685611947798,-0.153447990763203,
1.22044650153386));
#14469=CARTESIAN_POINT('Ctrl Pts',(0.0303468241642401,-0.143414812629152,
1.22309389090812));
#14470=CARTESIAN_POINT('Ctrl Pts',(0.0777622095232573,-0.133381634495101,
1.22574128028238));
#14471=CARTESIAN_POINT('Ctrl Pts',(0.119709190009594,-0.0975055458821257,
1.22838866965664));
#14472=CARTESIAN_POINT('Ctrl Pts',(0.136973893871985,-0.052219638220276,
1.2310360590309));
#14473=CARTESIAN_POINT('Ctrl Pts',(0.154238597734379,-0.00693373055842239,
1.23368344840516));
#14474=CARTESIAN_POINT('Ctrl Pts',(0.146821024972825,0.0477619961523044,
1.23633083777942));
#14475=CARTESIAN_POINT('Ctrl Pts',(0.118118804930222,0.0868140895256425,
1.23897822715368));
#14476=CARTESIAN_POINT('Ctrl Pts',(0.0894165848876198,0.125866182898978,
1.24162561652794));
#14477=CARTESIAN_POINT('Ctrl Pts',(0.0394297175639698,0.149274642934924,
1.2442730059022));
#14478=CARTESIAN_POINT('Ctrl Pts',(-0.00894524413350711,0.146317192515786,
1.24692039527646));
#14479=CARTESIAN_POINT('Ctrl Pts',(-0.0573202058309854,0.143359742096648,
1.24956778465072));
#14480=CARTESIAN_POINT('Ctrl Pts',(-0.104083261902292,0.114036381222425,
1.25221517402498));
#14481=CARTESIAN_POINT('Ctrl Pts',(-0.127814530591109,0.0717787154251623,
1.25486256339924));
#14482=CARTESIAN_POINT('Ctrl Pts',(-0.139981499518435,0.0501133037087236,
1.2562198740714));
#14483=CARTESIAN_POINT('Ctrl Pts',(-0.146094355379323,0.0250479932723348,
1.25757718474355));
#14484=CARTESIAN_POINT('Ctrl Pts',(-0.146109918970638,-1.0198006988139E-5,
1.25893449541571));
#14485=CARTESIAN_POINT('Origin',(0.,0.,0.));
#14486=CARTESIAN_POINT('',(-0.146470135615938,-0.000111966546850736,1.31606550458429));
#14487=CARTESIAN_POINT('',(-0.146410535958061,-0.000127756381200432,1.30893449541571));
#14488=CARTESIAN_POINT('',(-0.14635,-1.79227059055215E-17,0.));
#14489=CARTESIAN_POINT('Ctrl Pts',(-0.146470135615938,-0.000111966546850736,
1.31606550458429));
#14490=CARTESIAN_POINT('Ctrl Pts',(-0.146120207411574,0.0411799307449602,
1.31381483155218));
#14491=CARTESIAN_POINT('Ctrl Pts',(-0.127827491572984,0.0827431563937987,
1.31156415852007));
#14492=CARTESIAN_POINT('Ctrl Pts',(-0.0969137672218927,0.10998333351997,
1.30931348548796));
#14493=CARTESIAN_POINT('Ctrl Pts',(-0.0605655677022408,0.142012194937238,
1.30666715560886));
#14494=CARTESIAN_POINT('Ctrl Pts',(-0.00676890401288169,0.154239532672684,
1.30402082572976));
#14495=CARTESIAN_POINT('Ctrl Pts',(0.0398526445220406,0.14106870189023,
1.30137449585066));
#14496=CARTESIAN_POINT('Ctrl Pts',(0.0864741930569617,0.127897871107775,
1.29872816597155));
#14497=CARTESIAN_POINT('Ctrl Pts',(0.125920626437448,0.0893288718074177,
1.29608183609245));
#14498=CARTESIAN_POINT('Ctrl Pts',(0.14013669149516,0.0430153417578024,
1.29343550621335));
#14499=CARTESIAN_POINT('Ctrl Pts',(0.154352756552873,-0.00329818829181684,
1.29078917633425));
#14500=CARTESIAN_POINT('Ctrl Pts',(0.143338453287813,-0.0573562490906975,
1.28814284645515));
#14501=CARTESIAN_POINT('Ctrl Pts',(0.112135201594409,-0.0944156157243562,
1.28549651657604));
#14502=CARTESIAN_POINT('Ctrl Pts',(0.0809319499010078,-0.131474982358013,
1.28285018669694));
#14503=CARTESIAN_POINT('Ctrl Pts',(0.0295397497792676,-0.151535654826449,
1.28020385681784));
#14504=CARTESIAN_POINT('Ctrl Pts',(-0.0185183802362589,-0.1454155477333,
1.27755752693874));
#14505=CARTESIAN_POINT('Ctrl Pts',(-0.066576510251784,-0.139295440640151,
1.27491119705964));
#14506=CARTESIAN_POINT('Ctrl Pts',(-0.111300570161094,-0.106994553985419,
1.27226486718053));
#14507=CARTESIAN_POINT('Ctrl Pts',(-0.13221965410943,-0.0632975117719662,
1.26961853730143));
#14508=CARTESIAN_POINT('Ctrl Pts',(-0.141581826511298,-0.0437412423069929,
1.26843419306239));
#14509=CARTESIAN_POINT('Ctrl Pts',(-0.146176005022067,-0.0219023912433209,
1.26724984882334));
#14510=CARTESIAN_POINT('Ctrl Pts',(-0.146120596765396,-4.14129048147555E-5,
1.26606550458429));
#14511=CARTESIAN_POINT('Ctrl Pts',(-0.146109918970638,-1.0198006988139E-5,
1.25893449541571));
#14512=CARTESIAN_POINT('Ctrl Pts',(-0.146124711647138,-0.0238271763493914,
1.26022457411781));
#14513=CARTESIAN_POINT('Ctrl Pts',(-0.140631289159497,-0.0476377233371588,
1.26151465281992));
#14514=CARTESIAN_POINT('Ctrl Pts',(-0.129592576141605,-0.0685164391025303,
1.26280473152202));
#14515=CARTESIAN_POINT('Ctrl Pts',(-0.106939871696956,-0.111361957112663,
1.26545212089628));
#14516=CARTESIAN_POINT('Ctrl Pts',(-0.0609349815013302,-0.141861022412626,
1.26809951027054));
#14517=CARTESIAN_POINT('Ctrl Pts',(-0.0126505083952331,-0.146043496451057,
1.2707468996448));
#14518=CARTESIAN_POINT('Ctrl Pts',(0.0356339647108625,-0.150225970489488,
1.27339428901906));
#14519=CARTESIAN_POINT('Ctrl Pts',(0.0861980207274291,-0.128091853266388,
1.27604167839332));
#14520=CARTESIAN_POINT('Ctrl Pts',(0.11588072467734,-0.0897797074320025,
1.27868906776758));
#14521=CARTESIAN_POINT('Ctrl Pts',(0.145563428627253,-0.0514675615976161,
1.28133645714184));
#14522=CARTESIAN_POINT('Ctrl Pts',(0.154364780510509,0.00302261284805656,
1.2839838465161));
#14523=CARTESIAN_POINT('Ctrl Pts',(0.138253309066183,0.0487315170146188,
1.28663123589036));
#14524=CARTESIAN_POINT('Ctrl Pts',(0.122141837621857,0.0944404211811797,
1.28927862526462));
#14525=CARTESIAN_POINT('Ctrl Pts',(0.0811175428499519,0.131368055068631,
1.29192601463888));
#14526=CARTESIAN_POINT('Ctrl Pts',(0.0339716590485425,0.142599665496764,
1.29457340401314));
#14527=CARTESIAN_POINT('Ctrl Pts',(-0.013174224752867,0.153831275924897,
1.2972207933874));
#14528=CARTESIAN_POINT('Ctrl Pts',(-0.0664416975837803,0.139366862893713,
1.29986818276166));
#14529=CARTESIAN_POINT('Ctrl Pts',(-0.101431520699135,0.105831870563862,
1.30251557213592));
#14530=CARTESIAN_POINT('Ctrl Pts',(-0.129710573305276,0.0787286237393239,
1.30465521322918));
#14531=CARTESIAN_POINT('Ctrl Pts',(-0.146050663974784,0.0391684733249047,
1.30679485432245));
#14532=CARTESIAN_POINT('Ctrl Pts',(-0.146410535958061,-0.000127756381200432,
1.30893449541571));
#14533=CARTESIAN_POINT('Origin',(0.,0.,0.));
#14534=CARTESIAN_POINT('',(-0.146471469669193,0.000111495080380188,1.36606550458429));
#14535=CARTESIAN_POINT('',(-0.146526884620975,8.5711493927648E-5,1.35893449541571));
#14536=CARTESIAN_POINT('',(-0.14635,-1.79227059055215E-17,0.));
#14537=CARTESIAN_POINT('Ctrl Pts',(-0.146471469669193,0.000111495080380188,
1.36606550458429));
#14538=CARTESIAN_POINT('Ctrl Pts',(-0.146532402405025,0.0073220458586883,
1.36567247403923));
#14539=CARTESIAN_POINT('Ctrl Pts',(-0.146045973070864,0.0145243451116175,
1.36527944349416));
#14540=CARTESIAN_POINT('Ctrl Pts',(-0.144983764805735,0.0216407019395156,
1.3648864129491));
#14541=CARTESIAN_POINT('Ctrl Pts',(-0.137831767320671,0.0695561322809842,
1.36224008307));
#14542=CARTESIAN_POINT('Ctrl Pts',(-0.104576727819841,0.113575347233418,
1.3595937531909));
#14543=CARTESIAN_POINT('Ctrl Pts',(-0.060440002550743,0.133550058215342,
1.3569474233118));
#14544=CARTESIAN_POINT('Ctrl Pts',(-0.0163032772816473,0.153524769197265,
1.35430109343269));
#14545=CARTESIAN_POINT('Ctrl Pts',(0.0387151337557165,0.149454976208681,
1.35165476355359));
#14546=CARTESIAN_POINT('Ctrl Pts',(0.0794324390145508,0.123203488242689,
1.34900843367449));
#14547=CARTESIAN_POINT('Ctrl Pts',(0.120149744273387,0.0969520002766962,
1.34636210379539));
#14548=CARTESIAN_POINT('Ctrl Pts',(0.146565943753694,0.048518817333291,
1.34371577391629));
#14549=CARTESIAN_POINT('Ctrl Pts',(0.14658992694451,7.25688577880009E-5,
1.34106944403718));
#14550=CARTESIAN_POINT('Ctrl Pts',(0.146613910135327,-0.0483736796177136,
1.33842311415808));
#14551=CARTESIAN_POINT('Ctrl Pts',(0.120245677036657,-0.0968329936253116,
1.33577678427898));
#14552=CARTESIAN_POINT('Ctrl Pts',(0.0795543829983497,-0.123124782547022,
1.33313045439988));
#14553=CARTESIAN_POINT('Ctrl Pts',(0.0388630889600415,-0.149416571468734,
1.33048412452078));
#14554=CARTESIAN_POINT('Ctrl Pts',(-0.0161512660179049,-0.153540835304554,
1.32783779464168));
#14555=CARTESIAN_POINT('Ctrl Pts',(-0.0603077462478081,-0.133609833714981,
1.32519146476257));
#14556=CARTESIAN_POINT('Ctrl Pts',(-0.10446422647771,-0.113678832125408,
1.32254513488347));
#14557=CARTESIAN_POINT('Ctrl Pts',(-0.137762831959571,-0.0696925651104417,
1.31989880500437));
#14558=CARTESIAN_POINT('Ctrl Pts',(-0.144962267025529,-0.0217842390534145,
1.31725247512527));
#14559=CARTESIAN_POINT('Ctrl Pts',(-0.146038665626028,-0.0146213916011371,
1.31685681827827));
#14560=CARTESIAN_POINT('Ctrl Pts',(-0.146531651210624,-0.00737087161912708,
1.31646116143128));
#14561=CARTESIAN_POINT('Ctrl Pts',(-0.146470135615938,-0.000111966546850736,
1.31606550458429));
#14562=CARTESIAN_POINT('Ctrl Pts',(-0.146410535958061,-0.000127756381200432,
1.30893449541571));
#14563=CARTESIAN_POINT('Ctrl Pts',(-0.146495935505426,-0.00945296197092968,
1.30944224369671));
#14564=CARTESIAN_POINT('Ctrl Pts',(-0.145681427739287,-0.018763305174839,
1.3099499919777));
#14565=CARTESIAN_POINT('Ctrl Pts',(-0.143913007029536,-0.0278887903271487,
1.3104577402587));
#14566=CARTESIAN_POINT('Ctrl Pts',(-0.134692496844786,-0.0754688872597875,
1.31310512963296));
#14567=CARTESIAN_POINT('Ctrl Pts',(-0.0995393030754929,-0.118023509496548,
1.31575251900722));
#14568=CARTESIAN_POINT('Ctrl Pts',(-0.0545553941775042,-0.136060454153345,
1.31839990838148));
#14569=CARTESIAN_POINT('Ctrl Pts',(-0.00957148527951295,-0.154097398810142,
1.32104729775574));
#14570=CARTESIAN_POINT('Ctrl Pts',(0.0452431387471776,-0.14761666588697,
1.32369468713));
#14571=CARTESIAN_POINT('Ctrl Pts',(0.0847805644327026,-0.119586763955155,
1.32634207650426));
#14572=CARTESIAN_POINT('Ctrl Pts',(0.124317990118227,-0.09155686202334,
1.32898946587852));
#14573=CARTESIAN_POINT('Ctrl Pts',(0.148578217462589,-0.041977791082884,
1.33163685525278));
#14574=CARTESIAN_POINT('Ctrl Pts',(0.146448816178573,0.00644068764408242,
1.33428424462704));
#14575=CARTESIAN_POINT('Ctrl Pts',(0.144319414894557,0.0548591663710502,
1.3369316340013));
#14576=CARTESIAN_POINT('Ctrl Pts',(0.115800384982161,0.102117052884526,
1.33957902337556));
#14577=CARTESIAN_POINT('Ctrl Pts',(0.0739549070570988,0.126567807678519,
1.34222641274982));
#14578=CARTESIAN_POINT('Ctrl Pts',(0.0321094291320376,0.151018562472512,
1.34487380212408));
#14579=CARTESIAN_POINT('Ctrl Pts',(-0.0230624968056921,0.152662185547021,
1.34752119149834));
#14580=CARTESIAN_POINT('Ctrl Pts',(-0.0662892946253695,0.1307458130856,
1.3501685808726));
#14581=CARTESIAN_POINT('Ctrl Pts',(-0.109516092445046,0.10882944062418,
1.35281597024686));
#14582=CARTESIAN_POINT('Ctrl Pts',(-0.140797762146673,0.0633530726268328,
1.35546335962112));
#14583=CARTESIAN_POINT('Ctrl Pts',(-0.145805692234247,0.0151472216574969,
1.35811074899538));
#14584=CARTESIAN_POINT('Ctrl Pts',(-0.146325105122407,0.0101474034011793,
1.35838533113549));
#14585=CARTESIAN_POINT('Ctrl Pts',(-0.146561879835735,0.00511822289583405,
1.3586599132756));
#14586=CARTESIAN_POINT('Ctrl Pts',(-0.146526884620975,8.5711493927648E-5,
1.35893449541571));
#14587=CARTESIAN_POINT('Origin',(0.,0.,0.));
#14588=CARTESIAN_POINT('',(-0.146120987371435,4.2191387702159E-5,1.41606550458429));
#14589=CARTESIAN_POINT('',(-0.146148882937928,7.6306569664006E-5,1.40893449541571));
#14590=CARTESIAN_POINT('',(-0.14635,-1.79227059055215E-17,0.));
#14591=CARTESIAN_POINT('Ctrl Pts',(-0.146120987371435,4.2191387702159E-5,
1.41606550458429));
#14592=CARTESIAN_POINT('Ctrl Pts',(-0.146177309023295,0.021854523983563,
1.41488378664717));
#14593=CARTESIAN_POINT('Ctrl Pts',(-0.141604359564088,0.0436444172696427,
1.41370206871005));
#14594=CARTESIAN_POINT('Ctrl Pts',(-0.132282279973341,0.0631665524487371,
1.41252035077294));
#14595=CARTESIAN_POINT('Ctrl Pts',(-0.1114064880593,0.106884268839086,1.40987402089383));
#14596=CARTESIAN_POINT('Ctrl Pts',(-0.0667143915920224,0.139229456738304,
1.40722769101473));
#14597=CARTESIAN_POINT('Ctrl Pts',(-0.0186623352932378,0.145397151366753,
1.40458136113563));
#14598=CARTESIAN_POINT('Ctrl Pts',(0.0293897210055454,0.151564845995202,
1.40193503125653));
#14599=CARTESIAN_POINT('Ctrl Pts',(0.0808017371358351,0.131555047352884,
1.39928870137743));
#14600=CARTESIAN_POINT('Ctrl Pts',(0.112041660826149,0.0945265884816804,
1.39664237149832));
#14601=CARTESIAN_POINT('Ctrl Pts',(0.143281584516463,0.0574981296104763,
1.39399604161922));
#14602=CARTESIAN_POINT('Ctrl Pts',(0.154349415766802,0.00345101051038574,
1.39134971174012));
#14603=CARTESIAN_POINT('Ctrl Pts',(0.140179214932283,-0.0428765696854336,
1.38870338186102));
#14604=CARTESIAN_POINT('Ctrl Pts',(0.126009014097764,-0.089204149881253,
1.38605705198192));
#14605=CARTESIAN_POINT('Ctrl Pts',(0.0866007811783877,-0.127812191172801,
1.38341072210282));
#14606=CARTESIAN_POINT('Ctrl Pts',(0.0399922944706322,-0.14102917638501,
1.38076439222371));
#14607=CARTESIAN_POINT('Ctrl Pts',(-0.00661619223712474,-0.15424616159722,
1.37811806234461));
#14608=CARTESIAN_POINT('Ctrl Pts',(-0.060424932733261,-0.142072090730089,
1.37547173246551));
#14609=CARTESIAN_POINT('Ctrl Pts',(-0.0968048252466797,-0.110079232431271,
1.37282540258641));
#14610=CARTESIAN_POINT('Ctrl Pts',(-0.127781608685608,-0.08283792481198,
1.37057210325237));
#14611=CARTESIAN_POINT('Ctrl Pts',(-0.146122133733866,-0.0412276055847571,
1.36831880391833));
#14612=CARTESIAN_POINT('Ctrl Pts',(-0.146471469669193,0.000111495080380188,
1.36606550458429));
#14613=CARTESIAN_POINT('Ctrl Pts',(-0.146526884620975,8.5711493927648E-5,
1.35893449541571));
#14614=CARTESIAN_POINT('Ctrl Pts',(-0.146224472749943,-0.0434028397118431,
1.36130730264986));
#14615=CARTESIAN_POINT('Ctrl Pts',(-0.125627402569456,-0.0871401285467012,
1.36368010988401));
#14616=CARTESIAN_POINT('Ctrl Pts',(-0.0917490966422633,-0.114327780902106,
1.36605291711816));
#14617=CARTESIAN_POINT('Ctrl Pts',(-0.0539503804891888,-0.144661598551044,
1.36870030649242));
#14618=CARTESIAN_POINT('Ctrl Pts',(0.00038124229047478,-0.154393899907594,
1.37134769586668));
#14619=CARTESIAN_POINT('Ctrl Pts',(0.0463590973565905,-0.139066790892088,
1.37399508524094));
#14620=CARTESIAN_POINT('Ctrl Pts',(0.0923369524227062,-0.123739681876581,
1.3766424746152));
#14621=CARTESIAN_POINT('Ctrl Pts',(0.129961039775272,-0.083353162489017,
1.37928986398946));
#14622=CARTESIAN_POINT('Ctrl Pts',(0.141997595260484,-0.0364063334065561,
1.38193725336372));
#14623=CARTESIAN_POINT('Ctrl Pts',(0.154034150745695,0.0105404956759021,
1.38458464273798));
#14624=CARTESIAN_POINT('Ctrl Pts',(0.140483174363557,0.0640476344532581,
1.38723203211224));
#14625=CARTESIAN_POINT('Ctrl Pts',(0.10755170844225,0.0996060653705087,
1.3898794214865));
#14626=CARTESIAN_POINT('Ctrl Pts',(0.0746202425209409,0.135164496287762,
1.39252681086076));
#14627=CARTESIAN_POINT('Ctrl Pts',(0.0223082870604623,0.152774219344908,
1.39517420023502));
#14628=CARTESIAN_POINT('Ctrl Pts',(-0.025422593472234,0.144369075867769,
1.39782158960928));
#14629=CARTESIAN_POINT('Ctrl Pts',(-0.073153474004929,0.135963932390631,
1.40046897898354));
#14630=CARTESIAN_POINT('Ctrl Pts',(-0.11630327960984,0.101543922379208,
1.4031163683578));
#14631=CARTESIAN_POINT('Ctrl Pts',(-0.135107186188192,0.0568751802851974,
1.40576375773206));
#14632=CARTESIAN_POINT('Ctrl Pts',(-0.142614236437708,0.0390421576584788,
1.40682067029328));
#14633=CARTESIAN_POINT('Ctrl Pts',(-0.14624095998336,0.0195756595648056,
1.40787758285449));
#14634=CARTESIAN_POINT('Ctrl Pts',(-0.146148882937928,7.6306569664006E-5,
1.40893449541571));
#14635=CARTESIAN_POINT('Origin',(0.,0.,0.));
#14636=CARTESIAN_POINT('',(-0.14631473222987,-0.000131398079681141,1.46606550458429));
#14637=CARTESIAN_POINT('',(-0.146248097568756,-0.000123763188177425,1.45893449541571));
#14638=CARTESIAN_POINT('',(-0.14635,-1.79227059055215E-17,0.));
#14639=CARTESIAN_POINT('Ctrl Pts',(-0.14631473222987,-0.000131398079681141,
1.46606550458429));
#14640=CARTESIAN_POINT('Ctrl Pts',(-0.145989697979493,0.0361157155227289,
1.46409509925512));
#14641=CARTESIAN_POINT('Ctrl Pts',(-0.132370868650209,0.0725796635271419,
1.46212469392594));
#14642=CARTESIAN_POINT('Ctrl Pts',(-0.107973319296019,0.0991484059484618,
1.46015428859677));
#14643=CARTESIAN_POINT('Ctrl Pts',(-0.0752064754000165,0.134831245351468,
1.45750795871767));
#14644=CARTESIAN_POINT('Ctrl Pts',(-0.0229974942306327,0.152665588379184,
1.45486162883857));
#14645=CARTESIAN_POINT('Ctrl Pts',(0.0247535192036911,0.144485406820094,
1.45221529895946));
#14646=CARTESIAN_POINT('Ctrl Pts',(0.0725045326380122,0.136305225261004,
1.44956896908036));
#14647=CARTESIAN_POINT('Ctrl Pts',(0.115797578337275,0.102110519115111,
1.44692263920126));
#14648=CARTESIAN_POINT('Ctrl Pts',(0.134818450998255,0.0575543070937695,
1.44427630932216));
#14649=CARTESIAN_POINT('Ctrl Pts',(0.153839323659235,0.0129980950724284,
1.44162997944306));
#14650=CARTESIAN_POINT('Ctrl Pts',(0.148588023281934,-0.0419196228243577,
1.43898364956396));
#14651=CARTESIAN_POINT('Ctrl Pts',(0.121467255745355,-0.082062966762292,
1.43633731968485));
#14652=CARTESIAN_POINT('Ctrl Pts',(0.0943464882087764,-0.122206310700226,
1.43369098980575));
#14653=CARTESIAN_POINT('Ctrl Pts',(0.0453562535129183,-0.147575280679306,
1.43104465992665));
#14654=CARTESIAN_POINT('Ctrl Pts',(-0.00307937473935208,-0.146557666176543,
1.42839833004755));
#14655=CARTESIAN_POINT('Ctrl Pts',(-0.0515150029916225,-0.14554005167378,
1.42575200016845));
#14656=CARTESIAN_POINT('Ctrl Pts',(-0.0993960248003067,-0.118135852689175,
1.42310567028934));
#14657=CARTESIAN_POINT('Ctrl Pts',(-0.124806792024246,-0.0768886307561326,
1.42045934041024));
#14658=CARTESIAN_POINT('Ctrl Pts',(-0.138870387581649,-0.0540603453281256,
1.41899472846826));
#14659=CARTESIAN_POINT('Ctrl Pts',(-0.146051182757901,-0.0269918425378075,
1.41753011652627));
#14660=CARTESIAN_POINT('Ctrl Pts',(-0.146120987371435,4.2191387702159E-5,
1.41606550458429));
#14661=CARTESIAN_POINT('Ctrl Pts',(-0.146148882937928,7.6306569664006E-5,
1.40893449541571));
#14662=CARTESIAN_POINT('Ctrl Pts',(-0.146010322369016,-0.0292669616874671,
1.41052497222875));
#14663=CARTESIAN_POINT('Ctrl Pts',(-0.137450455640384,-0.0586846305953837,
1.4121154490418));
#14664=CARTESIAN_POINT('Ctrl Pts',(-0.121019719714466,-0.0827222215753489,
1.41370592585484));
#14665=CARTESIAN_POINT('Ctrl Pts',(-0.0936703391105966,-0.122733407165291,
1.4163533152291));
#14666=CARTESIAN_POINT('Ctrl Pts',(-0.0445135703510636,-0.147838304168576,
1.41900070460336));
#14667=CARTESIAN_POINT('Ctrl Pts',(0.00393424939099551,-0.146537573651384,
1.42164809397762));
#14668=CARTESIAN_POINT('Ctrl Pts',(0.0523820691330518,-0.145236843134192,
1.42429548335188));
#14669=CARTESIAN_POINT('Ctrl Pts',(0.100120939857634,-0.117530485096527,
1.42694287272614));
#14670=CARTESIAN_POINT('Ctrl Pts',(0.125284029446909,-0.0761094471358441,
1.4295902621004));
#14671=CARTESIAN_POINT('Ctrl Pts',(0.150447119036187,-0.0346884091751576,
1.43223765147466));
#14672=CARTESIAN_POINT('Ctrl Pts',(0.153034427490153,0.020447308708549,
1.43488504084892));
#14673=CARTESIAN_POINT('Ctrl Pts',(0.13186079120536,0.0640427391611241,
1.43753243022318));
#14674=CARTESIAN_POINT('Ctrl Pts',(0.110687154920568,0.107638169613697,
1.44017981959744));
#14675=CARTESIAN_POINT('Ctrl Pts',(0.0657525738970213,0.139693312635139,
1.4428272089717));
#14676=CARTESIAN_POINT('Ctrl Pts',(0.0176394768514684,0.145525221357757,
1.44547459834596));
#14677=CARTESIAN_POINT('Ctrl Pts',(-0.0304736201940859,0.151357130080375,
1.44812198772022));
#14678=CARTESIAN_POINT('Ctrl Pts',(-0.0817652332616461,0.130965804504167,
1.45076937709448));
#14679=CARTESIAN_POINT('Ctrl Pts',(-0.112741325423428,0.0936916042199666,
1.45341676646874));
#14680=CARTESIAN_POINT('Ctrl Pts',(-0.134261605244105,0.0677957870194472,
1.45525600945106));
#14681=CARTESIAN_POINT('Ctrl Pts',(-0.145976367207401,0.0337512577971725,
1.45709525243339));
#14682=CARTESIAN_POINT('Ctrl Pts',(-0.146248097568756,-0.000123763188177425,
1.45893449541571));
#14683=CARTESIAN_POINT('Origin',(0.,0.,-0.0924367114736175));
#14684=CARTESIAN_POINT('',(-0.117746618301147,-0.000105742458702955,1.48256328852638));
#14685=CARTESIAN_POINT('',(-0.117971241274414,-5.28325160115065E-6,1.49243671147361));
#14686=CARTESIAN_POINT('',(-0.117775,2.85464118895969E-14,-0.0924367114736175));
#14687=CARTESIAN_POINT('',(-0.117668597464313,0.00500517689812599,1.532225));
#14688=CARTESIAN_POINT('Ctrl Pts',(-0.117746618301147,-0.000105742458702949,
1.48256328852638));
#14689=CARTESIAN_POINT('Ctrl Pts',(-0.117836347163251,-0.0101121102621826,
1.48323921307631));
#14690=CARTESIAN_POINT('Ctrl Pts',(-0.112089674709738,-0.0591937430214443,
1.48656146750534));
#14691=CARTESIAN_POINT('Ctrl Pts',(-0.0435804807853106,-0.132222740314769,
1.49253005181348));
#14692=CARTESIAN_POINT('Ctrl Pts',(0.0874774386997331,-0.108286040948335,
1.50046904145078));
#14693=CARTESIAN_POINT('Ctrl Pts',(0.138385550162814,0.0147146982980264,
1.50840803108809));
#14694=CARTESIAN_POINT('Ctrl Pts',(0.0627460642121078,0.124368470664037,
1.51634702072539));
#14695=CARTESIAN_POINT('Ctrl Pts',(-0.0706026869052757,0.119928391791904,
1.5242860103627));
#14696=CARTESIAN_POINT('Ctrl Pts',(-0.116004137797729,0.0441355889673283,
1.5295786701209));
#14697=CARTESIAN_POINT('Ctrl Pts',(-0.117668597464313,0.00500517689812487,
1.532225));
#14698=CARTESIAN_POINT('',(-0.0334019664627544,0.1129391839063,1.53222500000001));
#14699=CARTESIAN_POINT('Origin',(0.,0.,1.532225));
#14700=CARTESIAN_POINT('Ctrl Pts',(-0.117971276761593,-5.28420699491729E-6,
1.49243671147361));
#14701=CARTESIAN_POINT('Ctrl Pts',(-0.117971582784674,-0.000385634193345565,
1.49246252744444));
#14702=CARTESIAN_POINT('Ctrl Pts',(-0.117794795258817,-0.0397700451254522,
1.49513573278954));
#14703=CARTESIAN_POINT('Ctrl Pts',(-0.0742871760264013,-0.117748889605885,
1.50045632750888));
#14704=CARTESIAN_POINT('Ctrl Pts',(0.0586284551779338,-0.126233948370975,
1.50839849563167));
#14705=CARTESIAN_POINT('Ctrl Pts',(0.137995068118234,-0.019163470063063,
1.51634066375444));
#14706=CARTESIAN_POINT('Ctrl Pts',(0.0906261803825392,0.105639137646141,
1.52428283187723));
#14707=CARTESIAN_POINT('Ctrl Pts',(0.00417072711528833,0.124051375507138,
1.52957761062575));
#14708=CARTESIAN_POINT('Ctrl Pts',(-0.0334019664627544,0.1129391839063,
1.53222500000001));
#14709=CARTESIAN_POINT('Origin',(0.,0.,-0.0924367114736175));
#14710=CARTESIAN_POINT('',(-0.117590702341447,3.3953472435133E-5,1.43256328852638));
#14711=CARTESIAN_POINT('',(-0.117692994131604,-9.95982882293356E-5,1.44243671147361));
#14712=CARTESIAN_POINT('',(-0.117775,2.85464118895969E-14,-0.0924367114736175));
#14713=CARTESIAN_POINT('Ctrl Pts',(-0.117590702341447,3.39534724351446E-5,
1.43256328852638));
#14714=CARTESIAN_POINT('Ctrl Pts',(-0.117534527156218,-0.0217216553118358,
1.43402790046837));
#14715=CARTESIAN_POINT('Ctrl Pts',(-0.101314495966545,-0.0828641818343832,
1.43813884228945));
#14716=CARTESIAN_POINT('Ctrl Pts',(-0.00292444232197888,-0.139176693688359,
1.44489611398964));
#14717=CARTESIAN_POINT('Ctrl Pts',(0.115350068603298,-0.0779297424218237,
1.45283510362695));
#14718=CARTESIAN_POINT('Ctrl Pts',(0.128028003046829,0.0546551750765237,
1.46077409326425));
#14719=CARTESIAN_POINT('Ctrl Pts',(0.0235079116789307,0.137209630484779,
1.46871308290156));
#14720=CARTESIAN_POINT('Ctrl Pts',(-0.0918059616614023,0.0978189523496558,
1.47597614798894));
#14721=CARTESIAN_POINT('Ctrl Pts',(-0.117485047349053,0.0290640819657798,
1.48059288319721));
#14722=CARTESIAN_POINT('Ctrl Pts',(-0.117746618301147,-0.000105742458702949,
1.48256328852638));
#14723=CARTESIAN_POINT('Ctrl Pts',(-0.117692994131604,-9.9598288229346E-5,
1.44243671147361));
#14724=CARTESIAN_POINT('Ctrl Pts',(-0.117789077779518,-0.0120777797952868,
1.44324485786555));
#14725=CARTESIAN_POINT('Ctrl Pts',(-0.110597905189529,-0.0631824179582176,
1.44670039363175));
#14726=CARTESIAN_POINT('Ctrl Pts',(-0.0368790902657646,-0.134252921254984,
1.45280331877221));
#14727=CARTESIAN_POINT('Ctrl Pts',(0.0928396680879532,-0.103751556080299,
1.46074548689499));
#14728=CARTESIAN_POINT('Ctrl Pts',(0.137511141307062,0.0217950526079239,
1.46868765501776));
#14729=CARTESIAN_POINT('Ctrl Pts',(0.0562018483347667,0.127378648737854,
1.47662982314055));
#14730=CARTESIAN_POINT('Ctrl Pts',(-0.0761502833827582,0.1162998103107,
1.48454617529249));
#14731=CARTESIAN_POINT('Ctrl Pts',(-0.117940200573233,0.0386186906477724,
1.48981513807018));
#14732=CARTESIAN_POINT('Ctrl Pts',(-0.117971276761593,-5.28420699491729E-6,
1.49243671147361));
#14733=CARTESIAN_POINT('Origin',(0.,0.,-0.0924367114736175));
#14734=CARTESIAN_POINT('',(-0.117872752581409,8.97255421561373E-5,1.38256328852638));
#14735=CARTESIAN_POINT('',(-0.117613151267609,6.14076272390171E-5,1.39243671147361));
#14736=CARTESIAN_POINT('',(-0.117775,2.85464118895969E-14,-0.0924367114736175));
#14737=CARTESIAN_POINT('Ctrl Pts',(-0.117872752581409,8.97255421561322E-5,
1.38256328852638));
#14738=CARTESIAN_POINT('Ctrl Pts',(-0.117591624875346,-0.0331778698171688,
1.38481658786042));
#14739=CARTESIAN_POINT('Ctrl Pts',(-0.0854981695600773,-0.105990339321694,
1.38971621707357));
#14740=CARTESIAN_POINT('Ctrl Pts',(0.0379781508110965,-0.133926497290667,
1.39726217616581));
#14741=CARTESIAN_POINT('Ctrl Pts',(0.133119345865688,-0.0407171622080862,
1.40520116580311));
#14742=CARTESIAN_POINT('Ctrl Pts',(0.106398871137127,0.0897659150453452,
1.41314015544042));
#14743=CARTESIAN_POINT('Ctrl Pts',(-0.0177224175491345,0.138074504763813,
1.42107914507772));
#14744=CARTESIAN_POINT('Ctrl Pts',(-0.105714817800915,0.0743914165933911,
1.42755352277305));
#14745=CARTESIAN_POINT('Ctrl Pts',(-0.11763602712824,0.0175874039095825,
1.43138157058926));
#14746=CARTESIAN_POINT('Ctrl Pts',(-0.117590702341447,3.39534724351446E-5,
1.43256328852638));
#14747=CARTESIAN_POINT('Ctrl Pts',(-0.117613151267609,6.1407627239024E-5,
1.39243671147361));
#14748=CARTESIAN_POINT('Ctrl Pts',(-0.117501644803633,-0.0235525549213426,
1.39402718828666));
#14749=CARTESIAN_POINT('Ctrl Pts',(-0.0991469449676741,-0.0866320980727062,
1.39826505447396));
#14750=CARTESIAN_POINT('Ctrl Pts',(0.00373660876362508,-0.139175849115243,
1.40515031003553));
#14751=CARTESIAN_POINT('Ctrl Pts',(0.118990018389619,-0.0722858665142316,
1.41309247815831));
#14752=CARTESIAN_POINT('Ctrl Pts',(0.125236419206141,0.0608253567263532,
1.42103464628109));
#14753=CARTESIAN_POINT('Ctrl Pts',(0.0167532566496359,0.13821437898841,
1.42897681440387));
#14754=CARTESIAN_POINT('Ctrl Pts',(-0.0944771051913143,0.0939940009069027,
1.43611083613471));
#14755=CARTESIAN_POINT('Ctrl Pts',(-0.117474319425011,0.0271612872365273,
1.44059746849129));
#14756=CARTESIAN_POINT('Ctrl Pts',(-0.117692994131604,-9.9598288229346E-5,
1.44243671147361));
#14757=CARTESIAN_POINT('Origin',(0.,0.,-0.0924367114736175));
#14758=CARTESIAN_POINT('',(-0.117871679003533,-9.01049542302267E-5,1.33256328852638));
#14759=CARTESIAN_POINT('',(-0.117917347702326,6.89762296073142E-5,1.34243671147361));
#14760=CARTESIAN_POINT('',(-0.117775,2.85464118895969E-14,-0.0924367114736175));
#14761=CARTESIAN_POINT('Ctrl Pts',(-0.117871679003533,-9.01049542302501E-5,
1.33256328852638));
#14762=CARTESIAN_POINT('Ctrl Pts',(-0.117921183610054,-0.00593170075121234,
1.33295894537338));
#14763=CARTESIAN_POINT('Ctrl Pts',(-0.114870949065289,-0.0507926200311143,
1.33600093209947));
#14764=CARTESIAN_POINT('Ctrl Pts',(-0.0572704544775333,-0.126880813469472,
1.34168924870467));
#14765=CARTESIAN_POINT('Ctrl Pts',(0.0755477687720905,-0.116923823242002,
1.34962823834197));
#14766=CARTESIAN_POINT('Ctrl Pts',(0.13920718769651,6.89141801743488E-5,
1.35756722797928));
#14767=CARTESIAN_POINT('Ctrl Pts',(0.0754319660950179,0.116998564767658,
1.36550621761658));
#14768=CARTESIAN_POINT('Ctrl Pts',(-0.0573960494825499,0.126824048933643,
1.37344520725389));
#14769=CARTESIAN_POINT('Ctrl Pts',(-0.11489462347839,0.0507140179075799,
1.37913089755716));
#14770=CARTESIAN_POINT('Ctrl Pts',(-0.117921788132912,0.00589240827474643,
1.38217025798132));
#14771=CARTESIAN_POINT('Ctrl Pts',(-0.117872752581409,8.97255421561322E-5,
1.38256328852638));
#14772=CARTESIAN_POINT('Ctrl Pts',(-0.117917347702326,6.89762296073276E-5,
1.34243671147361));
#14773=CARTESIAN_POINT('Ctrl Pts',(-0.117673982084908,-0.0349283870656527,
1.34480951870776));
#14774=CARTESIAN_POINT('Ctrl Pts',(-0.0826049238592893,-0.109396528181867,
1.34982971531618));
#14775=CARTESIAN_POINT('Ctrl Pts',(0.0440301174146577,-0.132080378229483,
1.35749730129884));
#14776=CARTESIAN_POINT('Ctrl Pts',(0.13486394497766,-0.0345773583278084,
1.36543946942163));
#14777=CARTESIAN_POINT('Ctrl Pts',(0.102148545386143,0.0946020732301706,
1.3733816375444));
#14778=CARTESIAN_POINT('Ctrl Pts',(-0.0241454188302812,0.137116288461919,
1.38132380566719));
#14779=CARTESIAN_POINT('Ctrl Pts',(-0.107458038693719,0.07065895059964,
1.38767549697692));
#14780=CARTESIAN_POINT('Ctrl Pts',(-0.117687250167678,0.015753490298928,
1.3913797989124));
#14781=CARTESIAN_POINT('Ctrl Pts',(-0.117613151267609,6.1407627239024E-5,
1.39243671147361));
#14782=CARTESIAN_POINT('Origin',(0.,0.,-0.0924367114736175));
#14783=CARTESIAN_POINT('',(-0.117590388001671,-3.33269891443968E-5,1.28256328852638));
#14784=CARTESIAN_POINT('',(-0.117823716245033,-0.000102811805890834,1.29243671147362));
#14785=CARTESIAN_POINT('',(-0.117775,2.85464118895969E-14,-0.0924367114736175));
#14786=CARTESIAN_POINT('Ctrl Pts',(-0.117590388001671,-3.33269891444124E-5,
1.28256328852638));
#14787=CARTESIAN_POINT('Ctrl Pts',(-0.117634977734708,-0.017625925033684,
1.28374763276543));
#14788=CARTESIAN_POINT('Ctrl Pts',(-0.105676786131388,-0.0744702911817869,
1.28757830688358));
#14789=CARTESIAN_POINT('Ctrl Pts',(-0.0175857351491984,-0.138091953858251,
1.29405531088083));
#14790=CARTESIAN_POINT('Ctrl Pts',(0.106487712804436,-0.089660542174548,
1.30199430051814));
#14791=CARTESIAN_POINT('Ctrl Pts',(0.133078957772855,0.0408489510387311,
1.30993329015544));
#14792=CARTESIAN_POINT('Ctrl Pts',(0.0378455373822902,0.133964029124136,
1.31787227979275));
#14793=CARTESIAN_POINT('Ctrl Pts',(-0.0855601048685178,0.105915403748908,
1.32541561258306));
#14794=CARTESIAN_POINT('Ctrl Pts',(-0.117590074669608,0.0331395035428114,
1.33031261549427));
#14795=CARTESIAN_POINT('Ctrl Pts',(-0.117871679003533,-9.01049542302501E-5,
1.33256328852638));
#14796=CARTESIAN_POINT('Ctrl Pts',(-0.117823716245033,-0.000102811805890825,
1.29243671147362));
#14797=CARTESIAN_POINT('Ctrl Pts',(-0.117892441435953,-0.00760726064997237,
1.29294445975461));
#14798=CARTESIAN_POINT('Ctrl Pts',(-0.113819337750002,-0.0541654333254181,
1.29609959740987));
#14799=CARTESIAN_POINT('Ctrl Pts',(-0.0518146499729274,-0.129225073214149,
1.30190212443939));
#14800=CARTESIAN_POINT('Ctrl Pts',(0.0805213734929343,-0.11357898534207,
1.30984429256217));
#14801=CARTESIAN_POINT('Ctrl Pts',(0.1390915465469,0.0061171215252809,1.31778646068495));
#14802=CARTESIAN_POINT('Ctrl Pts',(0.0702395735793815,0.120209316621791,
1.32572862880773));
#14803=CARTESIAN_POINT('Ctrl Pts',(-0.0629590648350173,0.124177428154433,
1.33367079693051));
#14804=CARTESIAN_POINT('Ctrl Pts',(-0.115917830154768,0.0471875384414626,
1.33924015781913));
#14805=CARTESIAN_POINT('Ctrl Pts',(-0.117945510062545,0.00411888419242175,
1.3421621293335));
#14806=CARTESIAN_POINT('Ctrl Pts',(-0.117917347702326,6.89762296073276E-5,
1.34243671147361));
#14807=CARTESIAN_POINT('Origin',(0.,0.,-0.0924367114736175));
#14808=CARTESIAN_POINT('',(-0.11774949833287,0.000107383800510985,1.23256328852638));
#14809=CARTESIAN_POINT('',(-0.117581795058195,-8.20683476789735E-6,1.24243671147361));
#14810=CARTESIAN_POINT('',(-0.117775,2.85464118895969E-14,-0.0924367114736175));
#14811=CARTESIAN_POINT('Ctrl Pts',(-0.11774949833287,0.000107383800510997,
1.23256328852638));
#14812=CARTESIAN_POINT('Ctrl Pts',(-0.1174869159147,-0.0291008736543001,
1.23453632015749));
#14813=CARTESIAN_POINT('Ctrl Pts',(-0.0917482398636095,-0.0978979247776974,
1.23915568166769));
#14814=CARTESIAN_POINT('Ctrl Pts',(0.0236422145726536,-0.137184880695923,
1.246421373057));
#14815=CARTESIAN_POINT('Ctrl Pts',(0.128082862902196,-0.0545291301253663,
1.2543603626943));
#14816=CARTESIAN_POINT('Ctrl Pts',(0.115272428336817,0.0780443019497631,
1.26229935233161));
#14817=CARTESIAN_POINT('Ctrl Pts',(-0.00306201423577413,0.139173524314926,
1.27023834196891));
#14818=CARTESIAN_POINT('Ctrl Pts',(-0.101358337705897,0.08278581645186,
1.27699298736717));
#14819=CARTESIAN_POINT('Ctrl Pts',(-0.117535345263889,0.02168343817453,
1.28110130288633));
#14820=CARTESIAN_POINT('Ctrl Pts',(-0.117590388001671,-3.33269891444124E-5,
1.28256328852638));
#14821=CARTESIAN_POINT('Ctrl Pts',(-0.117581795058195,-8.20683476789562E-6,
1.24243671147361));
#14822=CARTESIAN_POINT('Ctrl Pts',(-0.117593699448189,-0.0191748937105988,
1.24372679017572));
#14823=CARTESIAN_POINT('Ctrl Pts',(-0.104100832827715,-0.0776580224685839,
1.24766425825208));
#14824=CARTESIAN_POINT('Ctrl Pts',(-0.0120149744006178,-0.138706589206355,
1.25424911570271));
#14825=CARTESIAN_POINT('Ctrl Pts',(0.110059129405696,-0.0852693704304675,
1.26219128382548));
#14826=CARTESIAN_POINT('Ctrl Pts',(0.13130776387206,0.0462833517151888,
1.27013345194827));
#14827=CARTESIAN_POINT('Ctrl Pts',(0.0322649968732001,0.135435768819968,
1.27807562007105));
#14828=CARTESIAN_POINT('Ctrl Pts',(-0.0881142830049797,0.102747609761224,
1.28551003991283));
#14829=CARTESIAN_POINT('Ctrl Pts',(-0.117534109666069,0.0315207854174475,
1.29029707038035));
#14830=CARTESIAN_POINT('Ctrl Pts',(-0.117823716245033,-0.000102811805890825,
1.29243671147362));
#14831=CARTESIAN_POINT('Origin',(0.,0.,-0.0924367114736175));
#14832=CARTESIAN_POINT('',(-0.117957988745754,-3.12301727557783E-5,1.18256328852638));
#14833=CARTESIAN_POINT('',(-0.117793553451004,0.000106755881474893,1.19243671147362));
#14834=CARTESIAN_POINT('',(-0.117775,2.85464118895969E-14,-0.0924367114736175));
#14835=CARTESIAN_POINT('Ctrl Pts',(-0.117957988745754,-3.12301727557569E-5,
1.18256328852638));
#14836=CARTESIAN_POINT('Ctrl Pts',(-0.117964007145535,-0.00173159226684161,
1.18267867767044));
#14837=CARTESIAN_POINT('Ctrl Pts',(-0.117160216762375,-0.0424221720604921,
1.1854403966936));
#14838=CARTESIAN_POINT('Ctrl Pts',(-0.0703321751825429,-0.12013338809653,
1.19084844559586));
#14839=CARTESIAN_POINT('Ctrl Pts',(0.0627954496153871,-0.124239193932754,
1.19878743523316));
#14840=CARTESIAN_POINT('Ctrl Pts',(0.138438143943654,-0.0146125323915816,
1.20672642487047));
#14841=CARTESIAN_POINT('Ctrl Pts',(0.0873502052771435,0.108390901091839,
1.21466541450777));
#14842=CARTESIAN_POINT('Ctrl Pts',(-0.043700859820065,0.132169893139269,
1.22260440414508));
#14843=CARTESIAN_POINT('Ctrl Pts',(-0.112119660921406,0.0591163174148552,
1.22857036215128));
#14844=CARTESIAN_POINT('Ctrl Pts',(-0.117839104743291,0.0100747194789664,
1.23188999027838));
#14845=CARTESIAN_POINT('Ctrl Pts',(-0.11774949833287,0.000107383800510997,
1.23256328852638));
#14846=CARTESIAN_POINT('Ctrl Pts',(-0.117793553451004,0.000106755881474891,
1.19243671147362));
#14847=CARTESIAN_POINT('Ctrl Pts',(-0.117510050331475,-0.0305433296418112,
1.19450912059683));
#14848=CARTESIAN_POINT('Ctrl Pts',(-0.0896091397727994,-0.100804620014092,
1.19922891909429));
#14849=CARTESIAN_POINT('Ctrl Pts',(0.0288222657999454,-0.136209964735594,
1.20659610696603));
#14850=CARTESIAN_POINT('Ctrl Pts',(0.130092623711363,-0.0495962373069701,
1.21453827508881));
#14851=CARTESIAN_POINT('Ctrl Pts',(0.112184773380136,0.082452738709893,
1.22248044321158));
#14852=CARTESIAN_POINT('Ctrl Pts',(-0.00849585454694533,0.138966535376798,
1.23042261133437));
#14853=CARTESIAN_POINT('Ctrl Pts',(-0.103054997843392,0.079672038485689,
1.23707470075504));
#14854=CARTESIAN_POINT('Ctrl Pts',(-0.11756927027536,0.0201573447738481,
1.24107940080146));
#14855=CARTESIAN_POINT('Ctrl Pts',(-0.117581795058195,-8.20683476789562E-6,
1.24243671147361));
#14856=CARTESIAN_POINT('Origin',(0.,0.,-0.0924367114736175));
#14857=CARTESIAN_POINT('',(-0.117657565919426,-8.78585414499747E-5,1.13256328852638));
#14858=CARTESIAN_POINT('',(-0.117937823388479,-5.4172489969917E-5,1.14243671147362));
#14859=CARTESIAN_POINT('',(-0.117775,2.85464118895969E-14,-0.0924367114736175));
#14860=CARTESIAN_POINT('Ctrl Pts',(-0.117657565919426,-8.78585414499974E-5,
1.13256328852638));
#14861=CARTESIAN_POINT('Ctrl Pts',(-0.11775046973706,-0.0134980674796043,
1.13346736506249));
#14862=CARTESIAN_POINT('Ctrl Pts',(-0.109441032251172,-0.0660497484721492,
1.13701777147771));
#14863=CARTESIAN_POINT('Ctrl Pts',(-0.0320511128216771,-0.13546723577438,
1.14321450777202));
#14864=CARTESIAN_POINT('Ctrl Pts',(0.0964380908528195,-0.100390938007982,
1.15115349740933));
#14865=CARTESIAN_POINT('Ctrl Pts',(0.136644831685568,0.0265863832644056,
1.15909248704664));
#14866=CARTESIAN_POINT('Ctrl Pts',(0.0517625939920979,0.129225692742072,
1.16703147668394));
#14867=CARTESIAN_POINT('Ctrl Pts',(-0.0785823129332351,0.113795317289389,
1.17485507717719));
#14868=CARTESIAN_POINT('Ctrl Pts',(-0.117825981412732,0.0372644419932696,
1.18003234779134));
#14869=CARTESIAN_POINT('Ctrl Pts',(-0.117957988745754,-3.12301727557569E-5,
1.18256328852638));
#14870=CARTESIAN_POINT('Ctrl Pts',(-0.117937823388479,-5.41724899699178E-5,
1.14243671147362));
#14871=CARTESIAN_POINT('Ctrl Pts',(-0.117955293269658,-0.0031110520517566,
1.14264406164367));
#14872=CARTESIAN_POINT('Ctrl Pts',(-0.116460933142332,-0.0451799670343263,
1.14549880118799));
#14873=CARTESIAN_POINT('Ctrl Pts',(-0.0660858892268601,-0.122541963197144,
1.15100093010657));
#14874=CARTESIAN_POINT('Ctrl Pts',(0.0671705316110708,-0.121950798202395,
1.15894309822935));
#14875=CARTESIAN_POINT('Ctrl Pts',(0.138891844802359,-0.00964017357273747,
1.16688526635212));
#14876=CARTESIAN_POINT('Ctrl Pts',(0.0833739592533277,0.111501840422208,
1.17482743447491));
#14877=CARTESIAN_POINT('Ctrl Pts',(-0.0485230383040216,0.130496713571114,
1.18276960259768));
#14878=CARTESIAN_POINT('Ctrl Pts',(-0.113150295826959,0.0561813708375219,
1.18863936159726));
#14879=CARTESIAN_POINT('Ctrl Pts',(-0.117872210070015,0.00861047923971886,
1.19186173122257));
#14880=CARTESIAN_POINT('Ctrl Pts',(-0.117793553451004,0.000106755881474891,
1.19243671147362));
#14881=CARTESIAN_POINT('Origin',(0.,0.,-0.0924367114736175));
#14882=CARTESIAN_POINT('',(-0.117641451221435,8.0229283111194E-5,1.08256328852638));
#14883=CARTESIAN_POINT('',(-0.117630591849015,-7.42484764288953E-5,1.09243671147362));
#14884=CARTESIAN_POINT('',(-0.117775,2.85464118895969E-14,-0.0924367114736175));
#14885=CARTESIAN_POINT('Ctrl Pts',(-0.117641451221435,8.02292831111745E-5,
1.08256328852638));
#14886=CARTESIAN_POINT('Ctrl Pts',(-0.117483998834985,-0.0250372639622414,
1.08425605245455));
#14887=CARTESIAN_POINT('Ctrl Pts',(-0.0972946570053161,-0.0896524615425008,
1.08859514626182));
#14888=CARTESIAN_POINT('Ctrl Pts',(0.00904258428980543,-0.13891320121148,
1.09558056994819));
#14889=CARTESIAN_POINT('Ctrl Pts',(0.121617839487272,-0.067732908692211,
1.1035195595855));
#14890=CARTESIAN_POINT('Ctrl Pts',(0.122860297649024,0.0654522196953821,
1.1114585492228));
#14891=CARTESIAN_POINT('Ctrl Pts',(0.0116325734791967,0.138720326685422,
1.11939753886011));
#14892=CARTESIAN_POINT('Ctrl Pts',(-0.096364912740844,0.0911171059582243,
1.1264324519613));
#14893=CARTESIAN_POINT('Ctrl Pts',(-0.117478530206868,0.0257550656131636,
1.13082103518339));
#14894=CARTESIAN_POINT('Ctrl Pts',(-0.117657565919426,-8.78585414499974E-5,
1.13256328852638));
#14895=CARTESIAN_POINT('Ctrl Pts',(-0.117630591849015,-7.42484764288814E-5,
1.09243671147362));
#14896=CARTESIAN_POINT('Ctrl Pts',(-0.117715241483118,-0.0147626739157663,
1.09342639206478));
#14897=CARTESIAN_POINT('Ctrl Pts',(-0.108350501834675,-0.0686384992808382,
1.0970634620302));
#14898=CARTESIAN_POINT('Ctrl Pts',(-0.0276126195379174,-0.136460326620484,
1.10334792136989));
#14899=CARTESIAN_POINT('Ctrl Pts',(0.0997182217817603,-0.0971604536002107,
1.11129008949267));
#14900=CARTESIAN_POINT('Ctrl Pts',(0.135696927507188,0.0311483765905046,
1.11923225761545));
#14901=CARTESIAN_POINT('Ctrl Pts',(0.0473633069609982,0.130922093830007,
1.12717442573822));
#14902=CARTESIAN_POINT('Ctrl Pts',(-0.0809210029008042,0.111284164335459,
1.13490924369095));
#14903=CARTESIAN_POINT('Ctrl Pts',(-0.117732242679493,0.0359183370635313,
1.13999667226941));
#14904=CARTESIAN_POINT('Ctrl Pts',(-0.117937823388479,-5.41724899699178E-5,
1.14243671147362));
#14905=CARTESIAN_POINT('Origin',(0.,0.,-0.0924367114736175));
#14906=CARTESIAN_POINT('',(-0.117948158721073,4.38502512853227E-5,1.03256328852638));
#14907=CARTESIAN_POINT('',(-0.117667547954054,9.20194976846214E-5,1.04243671147362));
#14908=CARTESIAN_POINT('',(-0.117775,2.85464118895969E-14,-0.0924367114736175));
#14909=CARTESIAN_POINT('Ctrl Pts',(-0.117948158721073,4.38502512853157E-5,
1.03256328852638));
#14910=CARTESIAN_POINT('Ctrl Pts',(-0.117773439871091,-0.0365306738650768,
1.03504473984661));
#14911=CARTESIAN_POINT('Ctrl Pts',(-0.0798690478914953,-0.112422454385097,
1.04017252104593));
#14912=CARTESIAN_POINT('Ctrl Pts',(0.0493427524230464,-0.130168884856471,
1.04794663212436));
#14913=CARTESIAN_POINT('Ctrl Pts',(0.136125055048066,-0.0291310004912345,
1.05588562176166));
#14914=CARTESIAN_POINT('Ctrl Pts',(0.0982941990358779,0.0985743183458784,
1.06382461139897));
#14915=CARTESIAN_POINT('Ctrl Pts',(-0.0295182596522469,0.136041604476578,
1.07176360103627));
#14916=CARTESIAN_POINT('Ctrl Pts',(-0.108818061611988,0.067537217334308,
1.07800982674541));
#14917=CARTESIAN_POINT('Ctrl Pts',(-0.11773014713001,0.0142293884972668,
1.08160972257545));
#14918=CARTESIAN_POINT('Ctrl Pts',(-0.117641451221435,8.02292831111745E-5,
1.08256328852638));
#14919=CARTESIAN_POINT('Ctrl Pts',(-0.117667547954054,9.20194976846197E-5,
1.04243671147362));
#14920=CARTESIAN_POINT('Ctrl Pts',(-0.117475882803567,-0.0261866690710452,
1.04420872248589));
#14921=CARTESIAN_POINT('Ctrl Pts',(-0.0957916308421219,-0.0920126959480487,
1.04862812287242));
#14922=CARTESIAN_POINT('Ctrl Pts',(0.0132451643780021,-0.13859452774087,
1.05569491263321));
#14923=CARTESIAN_POINT('Ctrl Pts',(0.123654649330263,-0.0639797248987874,
1.06363708075599));
#14924=CARTESIAN_POINT('Ctrl Pts',(0.120783771971213,0.0692470788374567,
1.07157924887876));
#14925=CARTESIAN_POINT('Ctrl Pts',(0.00726255089817806,0.139036444335888,
1.07952141700155));
#14926=CARTESIAN_POINT('Ctrl Pts',(-0.0979368667310299,0.0886295245336828,
1.08647390453316));
#14927=CARTESIAN_POINT('Ctrl Pts',(-0.117488804242801,0.0245287720112504,
1.09077900269052));
#14928=CARTESIAN_POINT('Ctrl Pts',(-0.117630591849015,-7.42484764288814E-5,
1.09243671147362));
#14929=CARTESIAN_POINT('Origin',(0.,0.,-0.0924367114736175));
#14930=CARTESIAN_POINT('',(-0.117771476475648,-0.000107683352847938,0.982563288526384));
#14931=CARTESIAN_POINT('',(-0.11796176292438,2.53781033017321E-5,0.992436711473616));
#14932=CARTESIAN_POINT('',(-0.117775,2.85464118895969E-14,-0.0924367114736175));
#14933=CARTESIAN_POINT('Ctrl Pts',(-0.117771476475648,-0.000107683352847945,
0.982563288526384));
#14934=CARTESIAN_POINT('Ctrl Pts',(-0.117856103358663,-0.00933799346614349,
0.983187097359559));
#14935=CARTESIAN_POINT('Ctrl Pts',(-0.112646870919438,-0.057630810124202,
0.986457236071836));
#14936=CARTESIAN_POINT('Ctrl Pts',(-0.0461590140787468,-0.131331607851033,
0.992373704663214));
#14937=CARTESIAN_POINT('Ctrl Pts',(0.0853128637208732,-0.110001641284132,
1.00031269430052));
#14938=CARTESIAN_POINT('Ctrl Pts',(0.138686661656432,0.0120272889735618,
1.00825168393783));
#14939=CARTESIAN_POINT('Ctrl Pts',(0.0651023256631918,0.123046060459907,
1.01619067357513));
#14940=CARTESIAN_POINT('Ctrl Pts',(-0.0680787277209358,0.121424596492465,
1.02412966321244));
#14941=CARTESIAN_POINT('Ctrl Pts',(-0.116790117880403,0.0438975063746073,
1.02958720152952));
#14942=CARTESIAN_POINT('Ctrl Pts',(-0.11795976781127,0.00247402277930658,
1.0323984099675));
#14943=CARTESIAN_POINT('Ctrl Pts',(-0.117948158721073,4.38502512853157E-5,
1.03256328852638));
#14944=CARTESIAN_POINT('Ctrl Pts',(-0.11796176292438,2.53781033017319E-5,
0.992436711473616));
#14945=CARTESIAN_POINT('Ctrl Pts',(-0.117851518882229,-0.0376119105440478,
0.994991052906992));
#14946=CARTESIAN_POINT('Ctrl Pts',(-0.077958511321084,-0.114458475672252,
1.00019278371463));
#14947=CARTESIAN_POINT('Ctrl Pts',(0.0529591494285269,-0.128760265574912,
1.00804190389653));
#14948=CARTESIAN_POINT('Ctrl Pts',(0.136912761112491,-0.0252739657289669,
1.0159840720193));
#14949=CARTESIAN_POINT('Ctrl Pts',(0.0954402180350474,0.101365883217864,
1.02392624014209));
#14950=CARTESIAN_POINT('Ctrl Pts',(-0.0334653697086341,0.135144169424284,
1.03186840826486));
#14951=CARTESIAN_POINT('Ctrl Pts',(-0.109792739119276,0.0652029671457737,
1.03803856537538));
#14952=CARTESIAN_POINT('Ctrl Pts',(-0.117762231070763,0.0130737646421874,
1.04156133311163));
#14953=CARTESIAN_POINT('Ctrl Pts',(-0.117667547954054,9.20194976846197E-5,
1.04243671147362));
#14954=CARTESIAN_POINT('Origin',(0.,0.,-0.0924367114736175));
#14955=CARTESIAN_POINT('',(-0.117585265278523,2.16484251076657E-5,0.932563288526384));
#14956=CARTESIAN_POINT('',(-0.117742563953077,-0.000107211314308964,0.942436711473616));
#14957=CARTESIAN_POINT('',(-0.117775,2.85464118895969E-14,-0.0924367114736175));
#14958=CARTESIAN_POINT('Ctrl Pts',(-0.117585265278523,2.16484251076635E-5,
0.932563288526384));
#14959=CARTESIAN_POINT('Ctrl Pts',(-0.117550805757046,-0.0209622679161363,
0.933975784751614));
#14960=CARTESIAN_POINT('Ctrl Pts',(-0.102172791552808,-0.0813069697478888,
0.938034610855947));
#14961=CARTESIAN_POINT('Ctrl Pts',(-0.00565790085648466,-0.139092177922979,
0.944739766839381));
#14962=CARTESIAN_POINT('Ctrl Pts',(0.113796373024222,-0.0801812402497705,
0.952678756476687));
#14963=CARTESIAN_POINT('Ctrl Pts',(0.129077866376032,0.0521301276928276,
0.960617746113992));
#14964=CARTESIAN_POINT('Ctrl Pts',(0.026197419344502,0.13671993644362,0.968556735751298));
#14965=CARTESIAN_POINT('Ctrl Pts',(-0.0906967139502387,0.0993396518733501,
0.975871916555428));
#14966=CARTESIAN_POINT('Ctrl Pts',(-0.117497098103867,0.02981894716558,
0.980540767480457));
#14967=CARTESIAN_POINT('Ctrl Pts',(-0.117771476475648,-0.000107683352847945,
0.982563288526384));
#14968=CARTESIAN_POINT('Ctrl Pts',(-0.117742563953077,-0.000107211314308957,
0.942436711473616));
#14969=CARTESIAN_POINT('Ctrl Pts',(-0.117833632602859,-0.0103126986533654,
0.943125993953839));
#14970=CARTESIAN_POINT('Ctrl Pts',(-0.111944766202914,-0.0596118697348184,
0.946462665808322));
#14971=CARTESIAN_POINT('Ctrl Pts',(-0.0428565117498991,-0.132465832952297,
0.952446727037066));
#14972=CARTESIAN_POINT('Ctrl Pts',(0.0880997963686447,-0.107806787258123,
0.960388895159846));
#14973=CARTESIAN_POINT('Ctrl Pts',(0.138347640177547,0.0156143509765511,
0.968331063282625));
#14974=CARTESIAN_POINT('Ctrl Pts',(0.061854832590724,0.124731139593481,
0.976273231405407));
#14975=CARTESIAN_POINT('Ctrl Pts',(-0.0713033562375951,0.119581390225944,
0.984215399528185));
#14976=CARTESIAN_POINT('Ctrl Pts',(-0.117322772537986,0.0417718924351975,
0.989603226217589));
#14977=CARTESIAN_POINT('Ctrl Pts',(-0.11796577882491,0.00139640554830399,
0.992343663532733));
#14978=CARTESIAN_POINT('Ctrl Pts',(-0.11796176292438,2.53781033017319E-5,
0.992436711473616));
#14979=CARTESIAN_POINT('Origin',(0.,0.,-0.0924367114736175));
#14980=CARTESIAN_POINT('',(-0.117850913371472,9.6525574830472E-5,0.882563288526384));
#14981=CARTESIAN_POINT('',(-0.117591231449503,3.54948526558943E-5,0.892436711473616));
#14982=CARTESIAN_POINT('',(-0.117775,2.85464118895969E-14,-0.0924367114736175));
#14983=CARTESIAN_POINT('Ctrl Pts',(-0.117850913371472,9.65255748304767E-5,
0.882563288526384));
#14984=CARTESIAN_POINT('Ctrl Pts',(-0.117563006813672,-0.0324172738354332,
0.884764472143669));
#14985=CARTESIAN_POINT('Ctrl Pts',(-0.0867151192651892,-0.104499852648429,
0.889611985640057));
#14986=CARTESIAN_POINT('Ctrl Pts',(0.0353397195745277,-0.134646760160997,
0.897105829015547));
#14987=CARTESIAN_POINT('Ctrl Pts',(0.132293719443212,-0.0433245611326863,
0.905044818652852));
#14988=CARTESIAN_POINT('Ctrl Pts',(0.108141885842356,0.0876583043865096,
0.912983808290157));
#14989=CARTESIAN_POINT('Ctrl Pts',(-0.0150064327997127,0.138395999855801,
0.920922797927463));
#14990=CARTESIAN_POINT('Ctrl Pts',(-0.104951114476159,0.0759553573435841,
0.927449291339539));
#14991=CARTESIAN_POINT('Ctrl Pts',(-0.117615366114572,0.01835136974357,
0.931329454872513));
#14992=CARTESIAN_POINT('Ctrl Pts',(-0.117585265278523,2.16484251076635E-5,
0.932563288526384));
#14993=CARTESIAN_POINT('Ctrl Pts',(-0.117591231449503,3.54948526559117E-5,
0.892436711473616));
#14994=CARTESIAN_POINT('Ctrl Pts',(-0.117532234588281,-0.0218238662162972,
0.893908324374946));
#14995=CARTESIAN_POINT('Ctrl Pts',(-0.101194437785642,-0.0830895288483654,
0.898027326650536));
#14996=CARTESIAN_POINT('Ctrl Pts',(-0.00250162451743248,-0.139203517821528,
0.904793718300386));
#14997=CARTESIAN_POINT('Ctrl Pts',(0.115632500949424,-0.0775435504945224,
0.912735886423165));
#14998=CARTESIAN_POINT('Ctrl Pts',(0.127835376168433,0.0551542754370876,
0.920678054545947));
#14999=CARTESIAN_POINT('Ctrl Pts',(0.0229279137899797,0.137325118854324,
0.928620222668725));
#15000=CARTESIAN_POINT('Ctrl Pts',(-0.0920562790907298,0.0974788594069619,
0.935873108311283));
#15001=CARTESIAN_POINT('Ctrl Pts',(-0.117483857027998,0.0288844367965532,
0.94047860457958));
#15002=CARTESIAN_POINT('Ctrl Pts',(-0.117742563953077,-0.000107211314308957,
0.942436711473616));
#15003=CARTESIAN_POINT('Origin',(0.,0.,-0.0924367114736175));
#15004=CARTESIAN_POINT('',(-0.11789232318732,-8.18790992476613E-5,0.832563288526384));
#15005=CARTESIAN_POINT('',(-0.117872825429845,8.99519344067963E-5,0.842436711473616));
#15006=CARTESIAN_POINT('',(-0.117775,2.85464118895969E-14,-0.0924367114736175));
#15007=CARTESIAN_POINT('Ctrl Pts',(-0.11789232318732,-8.18790992476734E-5,
0.832563288526384));
#15008=CARTESIAN_POINT('Ctrl Pts',(-0.117932494517479,-0.00515170743829337,
0.832906829656623));
#15009=CARTESIAN_POINT('Ctrl Pts',(-0.115332713682068,-0.0492334187378749,
0.835896700665964));
#15010=CARTESIAN_POINT('Ctrl Pts',(-0.059752088941783,-0.125731196083361,
0.841532901554406));
#15011=CARTESIAN_POINT('Ctrl Pts',(0.0732361146625898,-0.118385460722959,
0.849471891191712));
#15012=CARTESIAN_POINT('Ctrl Pts',(0.139181674492094,-0.00266594955618734,
0.857410880829018));
#15013=CARTESIAN_POINT('Ctrl Pts',(0.077715950067195,0.115494055719818,
0.865349870466323));
#15014=CARTESIAN_POINT('Ctrl Pts',(-0.0548934004223171,0.127927168308903,
0.87328886010363));
#15015=CARTESIAN_POINT('Ctrl Pts',(-0.114416768398411,0.0522742940766184,
0.879026666123649));
#15016=CARTESIAN_POINT('Ctrl Pts',(-0.117909136832228,0.0066718045071592,
0.882118142264567));
#15017=CARTESIAN_POINT('Ctrl Pts',(-0.117850913371472,9.65255748304767E-5,
0.882563288526384));
#15018=CARTESIAN_POINT('Ctrl Pts',(-0.117872825429845,8.99519344067998E-5,
0.842436711473616));
#15019=CARTESIAN_POINT('Ctrl Pts',(-0.117591169542271,-0.0331870933343037,
0.844690654796053));
#15020=CARTESIAN_POINT('Ctrl Pts',(-0.0854771005934613,-0.106025606004136,
0.84959198749275));
#15021=CARTESIAN_POINT('Ctrl Pts',(0.0380692928980519,-0.133920149482284,
0.857140709563706));
#15022=CARTESIAN_POINT('Ctrl Pts',(0.133179650076608,-0.0405839661022353,
0.865082877686486));
#15023=CARTESIAN_POINT('Ctrl Pts',(0.106283765719693,0.0899312995767124,
0.873025045809266));
#15024=CARTESIAN_POINT('Ctrl Pts',(-0.0179789669825735,0.138060255849953,
0.880967213932046));
#15025=CARTESIAN_POINT('Ctrl Pts',(-0.105798194743126,0.0742290978659706,
0.887437769153496));
#15026=CARTESIAN_POINT('Ctrl Pts',(-0.117638368248411,0.0175004969839459,
0.891260935000686));
#15027=CARTESIAN_POINT('Ctrl Pts',(-0.117591231449503,3.54948526559117E-5,
0.892436711473616));
#15028=CARTESIAN_POINT('Origin',(0.,0.,-0.0924367114736175));
#15029=CARTESIAN_POINT('',(-0.117598114366551,-4.51832715892789E-5,0.782563288526384));
#15030=CARTESIAN_POINT('',(-0.117874685330111,-8.92836445515327E-5,0.792436711473617));
#15031=CARTESIAN_POINT('',(-0.117775,2.85464118895969E-14,-0.0924367114736175));
#15032=CARTESIAN_POINT('Ctrl Pts',(-0.117598114366551,-4.518327158929E-5,
0.782563288526384));
#15033=CARTESIAN_POINT('Ctrl Pts',(-0.117656123976761,-0.0168608793038394,
0.783695517048678));
#15034=CARTESIAN_POINT('Ctrl Pts',(-0.106420815930739,-0.0729055463807818,
0.787474075450074));
#15035=CARTESIAN_POINT('Ctrl Pts',(-0.0202952816069424,-0.137719814645367,
0.793898963730571));
#15036=CARTESIAN_POINT('Ctrl Pts',(0.104705698854998,-0.0917352845351548,
0.801837953367879));
#15037=CARTESIAN_POINT('Ctrl Pts',(0.133855787965376,0.0382266115373486,
0.809776943005182));
#15038=CARTESIAN_POINT('Ctrl Pts',(0.0404700769297216,0.133194664588195,
0.81771593264249));
#15039=CARTESIAN_POINT('Ctrl Pts',(-0.0843190215395119,0.107398870964955,
0.825311381149555));
#15040=CARTESIAN_POINT('Ctrl Pts',(-0.117623050954756,0.0339016606582783,
0.830260499777521));
#15041=CARTESIAN_POINT('Ctrl Pts',(-0.11789232318732,-8.18790992476734E-5,
0.832563288526384));
#15042=CARTESIAN_POINT('Ctrl Pts',(-0.117874685330111,-8.9283644551537E-5,
0.792436711473617));
#15043=CARTESIAN_POINT('Ctrl Pts',(-0.11792303416021,-0.00583050672374999,
0.7928255958429));
#15044=CARTESIAN_POINT('Ctrl Pts',(-0.114931453360353,-0.0506053896743902,
0.795861869586443));
#15045=CARTESIAN_POINT('Ctrl Pts',(-0.0575513573065257,-0.126774282767806,
0.801545532704245));
#15046=CARTESIAN_POINT('Ctrl Pts',(0.0753527000357912,-0.117071978271622,
0.809487700827026));
#15047=CARTESIAN_POINT('Ctrl Pts',(0.139225942868322,-0.000119714417332432,
0.817429868949805));
#15048=CARTESIAN_POINT('Ctrl Pts',(0.0755539188089132,0.116942220141962,
0.825372037072586));
#15049=CARTESIAN_POINT('Ctrl Pts',(-0.0573332568284509,0.12687306712048,
0.833314205195366));
#15050=CARTESIAN_POINT('Ctrl Pts',(-0.114890414736801,0.0507419104293215,
0.839002429995709));
#15051=CARTESIAN_POINT('Ctrl Pts',(-0.117921990994851,0.00589875908008548,
0.842043265421793));
#15052=CARTESIAN_POINT('Ctrl Pts',(-0.117872825429845,8.99519344067998E-5,
0.842436711473616));
#15053=CARTESIAN_POINT('Origin',(0.,0.,-0.0924367114736175));
#15054=CARTESIAN_POINT('',(-0.11772691567491,0.000105512987197037,0.732563288526384));
#15055=CARTESIAN_POINT('',(-0.117591850253004,-3.65476421498312E-5,0.742436711473616));
#15056=CARTESIAN_POINT('',(-0.117775,2.85464118895969E-14,-0.0924367114736175));
#15057=CARTESIAN_POINT('Ctrl Pts',(-0.11772691567491,0.000105512987197042,
0.732563288526384));
#15058=CARTESIAN_POINT('Ctrl Pts',(-0.117479624464894,-0.0283451130369189,
0.734484204440733));
#15059=CARTESIAN_POINT('Ctrl Pts',(-0.0928318426870313,-0.096374559506161,
0.739051450234184));
#15060=CARTESIAN_POINT('Ctrl Pts',(0.0209425314183671,-0.137622876656644,
0.746265025906738));
#15061=CARTESIAN_POINT('Ctrl Pts',(0.126986869252672,-0.0570349089493802,
0.754204015544043));
#15062=CARTESIAN_POINT('Ctrl Pts',(0.11678343126468,0.0757646090434518,
0.762143005181349));
#15063=CARTESIAN_POINT('Ctrl Pts',(-0.000327234354877375,0.139206819944772,
0.770081994818654));
#15064=CARTESIAN_POINT('Ctrl Pts',(-0.100479183608201,0.0843410365921374,
0.776888755933667));
#15065=CARTESIAN_POINT('Ctrl Pts',(-0.117520539541507,0.0224420334666934,
0.781049187169576));
#15066=CARTESIAN_POINT('Ctrl Pts',(-0.117598114366551,-4.518327158929E-5,
0.782563288526384));
#15067=CARTESIAN_POINT('Ctrl Pts',(-0.117591850253004,-3.65476421498364E-5,
0.742436711473616));
#15068=CARTESIAN_POINT('Ctrl Pts',(-0.117640211257931,-0.0174335619022046,
0.743607926264006));
#15069=CARTESIAN_POINT('Ctrl Pts',(-0.105863856762799,-0.0740921523660566,
0.747426530428656));
#15070=CARTESIAN_POINT('Ctrl Pts',(-0.0182163644075178,-0.138029133036789,
0.753892523967566));
#15071=CARTESIAN_POINT('Ctrl Pts',(0.106128952536144,-0.0901139441634624,
0.761834692090347));
#15072=CARTESIAN_POINT('Ctrl Pts',(0.133249245915149,0.0403548753208232,
0.769776860213125));
#15073=CARTESIAN_POINT('Ctrl Pts',(0.0382995408207276,0.133854483197375,
0.777719028335907));
#15074=CARTESIAN_POINT('Ctrl Pts',(-0.0853693283863186,0.106155717082476,
0.785272312089402));
#15075=CARTESIAN_POINT('Ctrl Pts',(-0.117593892160246,0.0332537408718532,
0.79017820646864));
#15076=CARTESIAN_POINT('Ctrl Pts',(-0.117874685330111,-8.9283644551537E-5,
0.792436711473617));
#15077=CARTESIAN_POINT('Origin',(0.,0.,-0.0924367114736175));
#15078=CARTESIAN_POINT('',(-0.117964947617991,-1.73329198795185E-5,0.682563288526384));
#15079=CARTESIAN_POINT('',(-0.117740574064672,0.000107068518266168,0.692436711473616));
#15080=CARTESIAN_POINT('',(-0.117775,2.85464118895969E-14,-0.0924367114736175));
#15081=CARTESIAN_POINT('Ctrl Pts',(-0.117964947617991,-1.73329198795367E-5,
0.682563288526384));
#15082=CARTESIAN_POINT('Ctrl Pts',(-0.117966864156947,-0.000949576032666658,
0.682626561953687));
#15083=CARTESIAN_POINT('Ctrl Pts',(-0.117534558560489,-0.0408698671952461,
0.685336165260092));
#15084=CARTESIAN_POINT('Ctrl Pts',(-0.0726787294560835,-0.118728463672822,
0.690692098445597));
#15085=CARTESIAN_POINT('Ctrl Pts',(0.0603425395611779,-0.125448888878168,
0.698631088082904));
#15086=CARTESIAN_POINT('Ctrl Pts',(0.138124349154501,-0.0173294538893964,
0.706570077720209));
#15087=CARTESIAN_POINT('Ctrl Pts',(0.0894627833767505,0.106653908470079,
0.714509067357515));
#15088=CARTESIAN_POINT('Ctrl Pts',(-0.0410958292974484,0.133002927094911,
0.72244805699482));
#15089=CARTESIAN_POINT('Ctrl Pts',(-0.111546724107196,0.0606813038481789,
0.728466130717777));
#15090=CARTESIAN_POINT('Ctrl Pts',(-0.117820302634623,0.0108495967181263,
0.731837874561632));
#15091=CARTESIAN_POINT('Ctrl Pts',(-0.11772691567491,0.000105512987197042,
0.732563288526384));
#15092=CARTESIAN_POINT('Ctrl Pts',(-0.117740574064672,0.000107068518266165,
0.692436711473616));
#15093=CARTESIAN_POINT('Ctrl Pts',(-0.117483171888848,-0.0288182833237499,
0.694390256685113));
#15094=CARTESIAN_POINT('Ctrl Pts',(-0.0921515028359353,-0.0973455904149804,
0.698991191270869));
#15095=CARTESIAN_POINT('Ctrl Pts',(0.022691720100341,-0.137364345221032,
0.706239515230886));
#15096=CARTESIAN_POINT('Ctrl Pts',(0.127740337615313,-0.0553740340325759,
0.714181683353665));
#15097=CARTESIAN_POINT('Ctrl Pts',(0.115765682611161,0.077344581120379,
0.722123851476446));
#15098=CARTESIAN_POINT('Ctrl Pts',(-0.00226223072526165,0.139207614056346,
0.730066019599226));
#15099=CARTESIAN_POINT('Ctrl Pts',(-0.101117998472899,0.083225715609228,
0.736836972931616));
#15100=CARTESIAN_POINT('Ctrl Pts',(-0.117530897055598,0.0218902846491045,
0.740960536889746));
#15101=CARTESIAN_POINT('Ctrl Pts',(-0.117591850253004,-3.65476421498364E-5,
0.742436711473616));
#15102=CARTESIAN_POINT('Origin',(0.,0.,-0.0924367114736175));
#15103=CARTESIAN_POINT('',(-0.117676160015555,-9.46906955630148E-5,0.632563288526383));
#15104=CARTESIAN_POINT('',(-0.117962383120995,-2.41598447144192E-5,0.642436711473616));
#15105=CARTESIAN_POINT('',(-0.117775,2.85464118895969E-14,-0.0924367114736175));
#15106=CARTESIAN_POINT('Ctrl Pts',(-0.117676160015555,-9.46906955630045E-5,
0.632563288526383));
#15107=CARTESIAN_POINT('Ctrl Pts',(-0.117771520970562,-0.0127268345011372,
0.633415249345741));
#15108=CARTESIAN_POINT('Ctrl Pts',(-0.110078248258936,-0.064483421762156,
0.636913540044201));
#15109=CARTESIAN_POINT('Ctrl Pts',(-0.0347063025259737,-0.134811417789573,
0.643058160621763));
#15110=CARTESIAN_POINT('Ctrl Pts',(0.0944472082050275,-0.102266175560326,
0.65099715025907));
#15111=CARTESIAN_POINT('Ctrl Pts',(0.137140772714236,0.0238967416356601,
0.658936139896373));
#15112=CARTESIAN_POINT('Ctrl Pts',(0.054291358674537,0.128183829614862,
0.666875129533682));
#15113=CARTESIAN_POINT('Ctrl Pts',(-0.0772016597727435,0.11523146575827,
0.674750845743682));
#15114=CARTESIAN_POINT('Ctrl Pts',(-0.117886707375211,0.0380402955314478,
0.679980232074585));
#15115=CARTESIAN_POINT('Ctrl Pts',(-0.117964947617991,-1.73329198795367E-5,
0.682563288526384));
#15116=CARTESIAN_POINT('Ctrl Pts',(-0.117962383120995,-2.41598447144253E-5,
0.642436711473616));
#15117=CARTESIAN_POINT('Ctrl Pts',(-0.117966033213387,-0.0013279541977536,
0.642525197731959));
#15118=CARTESIAN_POINT('Ctrl Pts',(-0.117355585052125,-0.0416360146359673,
0.645261073364563));
#15119=CARTESIAN_POINT('Ctrl Pts',(-0.0715088964667609,-0.119458592094588,
0.650644338371427));
#15120=CARTESIAN_POINT('Ctrl Pts',(0.0616402393688536,-0.124837327709565,
0.658586506494205));
#15121=CARTESIAN_POINT('Ctrl Pts',(0.138320583400205,-0.0158522461166236,
0.666528674616987));
#15122=CARTESIAN_POINT('Ctrl Pts',(0.0882850628235238,0.107655121482266,
0.674470842739765));
#15123=CARTESIAN_POINT('Ctrl Pts',(-0.0426286451686149,0.132539337972556,
0.682413010862546));
#15124=CARTESIAN_POINT('Ctrl Pts',(-0.111894847147975,0.059748848130285,
0.68840163377383));
#15125=CARTESIAN_POINT('Ctrl Pts',(-0.117831996057943,0.0103805377030848,
0.691742867310853));
#15126=CARTESIAN_POINT('Ctrl Pts',(-0.117740574064672,0.000107068518266165,
0.692436711473616));
#15127=CARTESIAN_POINT('Origin',(0.,0.,-0.0924367114736175));
#15128=CARTESIAN_POINT('',(-0.117626285855324,7.11112359239178E-5,0.582563288526384));
#15129=CARTESIAN_POINT('',(-0.11766919235599,-9.26074537421634E-5,0.592436711473616));
#15130=CARTESIAN_POINT('',(-0.117775,2.85464118895969E-14,-0.0924367114736175));
#15131=CARTESIAN_POINT('Ctrl Pts',(-0.117626285855324,7.11112359239024E-5,
0.582563288526383));
#15132=CARTESIAN_POINT('Ctrl Pts',(-0.117492102008102,-0.0242809575267813,
0.584203936737797));
#15133=CARTESIAN_POINT('Ctrl Pts',(-0.0982512120079041,-0.0881067492982899,
0.588490914828312));
#15134=CARTESIAN_POINT('Ctrl Pts',(0.00631176444456456,-0.139064040754811,
0.595424222797929));
#15135=CARTESIAN_POINT('Ctrl Pts',(0.120263693490807,-0.0701091280034811,
0.603363212435234));
#15136=CARTESIAN_POINT('Ctrl Pts',(0.124122453355413,0.0630258865426945,
0.611302202072541));
#15137=CARTESIAN_POINT('Ctrl Pts',(0.0143556138404206,0.138465021405133,
0.619241191709845));
#15138=CARTESIAN_POINT('Ctrl Pts',(-0.0953630726970595,0.0926558297308384,
0.626328220527794));
#15139=CARTESIAN_POINT('Ctrl Pts',(-0.117475314221613,0.0265106736450616,
0.630768919466639));
#15140=CARTESIAN_POINT('Ctrl Pts',(-0.117676160015555,-9.46906955630045E-5,
0.632563288526383));
#15141=CARTESIAN_POINT('Ctrl Pts',(-0.11766919235599,-9.26074537421669E-5,
0.592436711473616));
#15142=CARTESIAN_POINT('Ctrl Pts',(-0.117764072896019,-0.0130062487266101,
0.593307528153066));
#15143=CARTESIAN_POINT('Ctrl Pts',(-0.109848366281979,-0.0650658641993071,
0.596825734206776));
#15144=CARTESIAN_POINT('Ctrl Pts',(-0.0336977294021144,-0.135086418755761,
0.602991329634746));
#15145=CARTESIAN_POINT('Ctrl Pts',(0.0952657566843092,-0.101529863106778,
0.610933497757526));
#15146=CARTESIAN_POINT('Ctrl Pts',(0.136956022624868,0.025038477707157,
0.618875665880307));
#15147=CARTESIAN_POINT('Ctrl Pts',(0.0531805018142573,0.128669000640787,
0.626817834003085));
#15148=CARTESIAN_POINT('Ctrl Pts',(-0.0778376600742765,0.114584191752874,
0.634671515867523));
#15149=CARTESIAN_POINT('Ctrl Pts',(-0.117856827377429,0.0376798124439797,
0.639877808357699));
#15150=CARTESIAN_POINT('Ctrl Pts',(-0.117962383120995,-2.41598447144253E-5,
0.642436711473616));
#15151=CARTESIAN_POINT('Origin',(0.,0.,-0.0924367114736175));
#15152=CARTESIAN_POINT('',(-0.117934829819181,5.63106208242181E-5,0.532563288526383));
#15153=CARTESIAN_POINT('',(-0.117629301205424,7.34277634442948E-5,0.542436711473615));
#15154=CARTESIAN_POINT('',(-0.117775,2.85464118895969E-14,-0.0924367114736175));
#15155=CARTESIAN_POINT('Ctrl Pts',(-0.117934829819181,5.63106208242166E-5,
0.532563288526383));
#15156=CARTESIAN_POINT('Ctrl Pts',(-0.117723349859012,-0.0357608023914865,
0.534992624129852));
#15157=CARTESIAN_POINT('Ctrl Pts',(-0.0811985738067347,-0.110967619805887,
0.540068289612422));
#15158=CARTESIAN_POINT('Ctrl Pts',(0.0467759446245483,-0.131113145053959,
0.547790284974095));
#15159=CARTESIAN_POINT('Ctrl Pts',(0.135526478334676,-0.031799677225719,
0.555729274611401));
#15160=CARTESIAN_POINT('Ctrl Pts',(0.100211809365564,0.0966242157284558,
0.563668264248707));
#15161=CARTESIAN_POINT('Ctrl Pts',(-0.0268399031138932,0.136595261273209,
0.571607253886012));
#15162=CARTESIAN_POINT('Ctrl Pts',(-0.108142973925314,0.0691035501437442,
0.577905595311905));
#15163=CARTESIAN_POINT('Ctrl Pts',(-0.117708537635025,0.0149983997031143,
0.581557606858695));
#15164=CARTESIAN_POINT('Ctrl Pts',(-0.117626285855324,7.11112359239024E-5,
0.582563288526383));
#15165=CARTESIAN_POINT('Ctrl Pts',(-0.117629301205424,7.34277634442983E-5,
0.542436711473615));
#15166=CARTESIAN_POINT('Ctrl Pts',(-0.11748956090956,-0.0244625652698295,
0.544089858574172));
#15167=CARTESIAN_POINT('Ctrl Pts',(-0.0980201725405651,-0.0884941619373469,
0.548390395048989));
#15168=CARTESIAN_POINT('Ctrl Pts',(0.00702343738442799,-0.139048728244533,
0.555338320898066));
#15169=CARTESIAN_POINT('Ctrl Pts',(0.12066450826877,-0.0694546898587181,
0.563280489020846));
#15170=CARTESIAN_POINT('Ctrl Pts',(0.123764493242992,0.063766979789076,
0.571222657143626));
#15171=CARTESIAN_POINT('Ctrl Pts',(0.0134834875971477,0.13857154491934,
0.579164825266405));
#15172=CARTESIAN_POINT('Ctrl Pts',(-0.0957036897026042,0.092147346049863,
0.586236176709736));
#15173=CARTESIAN_POINT('Ctrl Pts',(-0.117475624432153,0.0262528025703711,
0.590660138778806));
#15174=CARTESIAN_POINT('Ctrl Pts',(-0.11766919235599,-9.26074537421669E-5,
0.592436711473616));
#15175=CARTESIAN_POINT('Origin',(0.,0.,-0.0924367114736175));
#15176=CARTESIAN_POINT('',(-0.117794891956694,-0.000106411733115368,0.482563288526384));
#15177=CARTESIAN_POINT('',(-0.117936566864074,5.52347650140707E-5,0.492436711473616));
#15178=CARTESIAN_POINT('',(-0.117775,2.85464118895969E-14,-0.0924367114736175));
#15179=CARTESIAN_POINT('Ctrl Pts',(-0.117794891956694,-0.000106411733115381,
0.482563288526384));
#15180=CARTESIAN_POINT('Ctrl Pts',(-0.117872998614688,-0.00856127641466401,
0.483134981642805));
#15181=CARTESIAN_POINT('Ctrl Pts',(-0.113184542395844,-0.0560672187853419,
0.486353004638329));
#15182=CARTESIAN_POINT('Ctrl Pts',(-0.0487302328423073,-0.130399425645183,
0.492217357512954));
#15183=CARTESIAN_POINT('Ctrl Pts',(0.0831353173341669,-0.111656458896056,
0.50015634715026));
#15184=CARTESIAN_POINT('Ctrl Pts',(0.13889618212661,0.00930034365552528,
0.508095336787567));
#15185=CARTESIAN_POINT('Ctrl Pts',(0.0675071113591811,0.12174331898465,
0.516034326424871));
#15186=CARTESIAN_POINT('Ctrl Pts',(-0.0656800932930844,0.122738629397884,
0.523973316062178));
#15187=CARTESIAN_POINT('Ctrl Pts',(-0.116384786286051,0.04545243224792,
0.529482970096015));
#15188=CARTESIAN_POINT('Ctrl Pts',(-0.117953719733239,0.00325558390455253,
0.53234629425075));
#15189=CARTESIAN_POINT('Ctrl Pts',(-0.117934829819181,5.63106208242166E-5,
0.532563288526383));
#15190=CARTESIAN_POINT('Ctrl Pts',(-0.117936566864074,5.52347650140663E-5,
0.492436711473616));
#15191=CARTESIAN_POINT('Ctrl Pts',(-0.117728017843002,-0.0358510361847084,
0.494872188995279));
#15192=CARTESIAN_POINT('Ctrl Pts',(-0.0810366231971402,-0.111156550628637,
0.499955055891203));
#15193=CARTESIAN_POINT('Ctrl Pts',(0.0471380885036503,-0.131003351527116,
0.507685312161385));
#15194=CARTESIAN_POINT('Ctrl Pts',(0.135643160584381,-0.031381690295376,
0.515627480284167));
#15195=CARTESIAN_POINT('Ctrl Pts',(0.0998851624184703,0.0969888232104648,
0.523569648406945));
#15196=CARTESIAN_POINT('Ctrl Pts',(-0.0273779061153799,0.136507610615132,
0.531511816529727));
#15197=CARTESIAN_POINT('Ctrl Pts',(-0.108290992649607,0.0687756007668377,
0.537800837551949));
#15198=CARTESIAN_POINT('Ctrl Pts',(-0.117713344367368,0.0148299618267192,
0.541442469199912));
#15199=CARTESIAN_POINT('Ctrl Pts',(-0.117629301205424,7.34277634442983E-5,
0.542436711473615));
#15200=CARTESIAN_POINT('Origin',(0.,0.,-0.0924367114736175));
#15201=CARTESIAN_POINT('',(-0.117582256074849,9.06819982020624E-6,0.432563288526383));
#15202=CARTESIAN_POINT('',(-0.11779560903417,-0.000106574656651148,0.442436711473616));
#15203=CARTESIAN_POINT('',(-0.117775,2.85464118895969E-14,-0.0924367114736175));
#15204=CARTESIAN_POINT('Ctrl Pts',(-0.117582256074849,9.06819982019261E-6,
0.432563288526383));
#15205=CARTESIAN_POINT('Ctrl Pts',(-0.117568373935691,-0.020201912089319,
0.43392366903486));
#15206=CARTESIAN_POINT('Ctrl Pts',(-0.10300922874285,-0.0797477867736473,
0.437930379422439));
#15207=CARTESIAN_POINT('Ctrl Pts',(-0.00838939967687663,-0.138954178686792,
0.44458341968912));
#15208=CARTESIAN_POINT('Ctrl Pts',(0.11219917790857,-0.0824013973067221,
0.452522409326426));
#15209=CARTESIAN_POINT('Ctrl Pts',(0.13007709763057,0.0495842159710775,
0.460461398963732));
#15210=CARTESIAN_POINT('Ctrl Pts',(0.0288783492374893,0.136178877755608,
0.468400388601037));
#15211=CARTESIAN_POINT('Ctrl Pts',(-0.0895654556576369,0.100852400902523,
0.475767685121922));
#15212=CARTESIAN_POINT('Ctrl Pts',(-0.117511448025972,0.0305757367622385,
0.480488651763704));
#15213=CARTESIAN_POINT('Ctrl Pts',(-0.117794891956694,-0.000106411733115381,
0.482563288526384));
#15214=CARTESIAN_POINT('Ctrl Pts',(-0.11779560903417,-0.000106574656651151,
0.442436711473616));
#15215=CARTESIAN_POINT('Ctrl Pts',(-0.117873644338608,-0.00854245500997505,
0.443007130042126));
#15216=CARTESIAN_POINT('Ctrl Pts',(-0.113196618671047,-0.056044542179559,
0.446224937984896));
#15217=CARTESIAN_POINT('Ctrl Pts',(-0.0487473834415776,-0.130413074907061,
0.452090135301926));
#15218=CARTESIAN_POINT('Ctrl Pts',(0.0831820848081396,-0.111645054821459,
0.460032303424706));
#15219=CARTESIAN_POINT('Ctrl Pts',(0.138908217753341,0.00940130521287039,
0.467974471547486));
#15220=CARTESIAN_POINT('Ctrl Pts',(0.0673801526530663,0.121835103839429,
0.475916639670265));
#15221=CARTESIAN_POINT('Ctrl Pts',(-0.0658750545035054,0.12265543075329,
0.483858807793047));
#15222=CARTESIAN_POINT('Ctrl Pts',(-0.116424939330292,0.0453161125527027,
0.489365498394162));
#15223=CARTESIAN_POINT('Ctrl Pts',(-0.11795471279604,0.00317945345687678,
0.492224799621019));
#15224=CARTESIAN_POINT('Ctrl Pts',(-0.117936566864074,5.52347650140663E-5,
0.492436711473616));
#15225=CARTESIAN_POINT('Origin',(0.,0.,-0.0924367114736175));
#15226=CARTESIAN_POINT('',(-0.117828183671793,0.000101754196006455,0.382563288526383));
#15227=CARTESIAN_POINT('',(-0.117581664177921,7.09484545444172E-6,0.392436711473616));
#15228=CARTESIAN_POINT('',(-0.117775,2.85464118895969E-14,-0.0924367114736175));
#15229=CARTESIAN_POINT('Ctrl Pts',(-0.117828183671793,0.000101754196006446,
0.382563288526384));
#15230=CARTESIAN_POINT('Ctrl Pts',(-0.117538790254565,-0.0316580736410773,
0.384712356426916));
#15231=CARTESIAN_POINT('Ctrl Pts',(-0.0879068326507716,-0.103002379129266,
0.38950775420655));
#15232=CARTESIAN_POINT('Ctrl Pts',(0.0326876424682324,-0.135315053971568,
0.396949481865287));
#15233=CARTESIAN_POINT('Ctrl Pts',(0.13141703692502,-0.0459152284901983,
0.404888471502591));
#15234=CARTESIAN_POINT('Ctrl Pts',(0.109843140674695,0.0855168418978295,
0.412827461139898));
#15235=CARTESIAN_POINT('Ctrl Pts',(-0.0122846228212416,0.13866410438033,
0.420766450777203));
#15236=CARTESIAN_POINT('Ctrl Pts',(-0.104166535924894,0.0775181589932739,
0.427345059906032));
#15237=CARTESIAN_POINT('Ctrl Pts',(-0.117595378674006,0.0191142356295008,
0.431277339155758));
#15238=CARTESIAN_POINT('Ctrl Pts',(-0.117582256074849,9.06819982019261E-6,
0.432563288526383));
#15239=CARTESIAN_POINT('Ctrl Pts',(-0.117581664177921,7.09484545444172E-6,
0.392436711473616));
#15240=CARTESIAN_POINT('Ctrl Pts',(-0.117570873504463,-0.0200907396801347,
0.393789460463232));
#15241=CARTESIAN_POINT('Ctrl Pts',(-0.10312708440739,-0.079535468422451,
0.397789598827109));
#15242=CARTESIAN_POINT('Ctrl Pts',(-0.00873482453528946,-0.138951719454826,
0.404437126565246));
#15243=CARTESIAN_POINT('Ctrl Pts',(0.112042812448737,-0.0826455423945668,
0.412379294688026));
#15244=CARTESIAN_POINT('Ctrl Pts',(0.130177722634257,0.049372441998279,
0.420321462810806));
#15245=CARTESIAN_POINT('Ctrl Pts',(0.0290564652212241,0.136160197297018,
0.428263630933586));
#15246=CARTESIAN_POINT('Ctrl Pts',(-0.0895090212855029,0.100936776489487,
0.435635380487856));
#15247=CARTESIAN_POINT('Ctrl Pts',(-0.117511471984497,0.0306096014671689,
0.440359740667866));
#15248=CARTESIAN_POINT('Ctrl Pts',(-0.11779560903417,-0.000106574656651151,
0.442436711473616));
#15249=CARTESIAN_POINT('Origin',(0.,0.,-0.0924367114736175));
#15250=CARTESIAN_POINT('',(-0.117911328466355,-7.22474488887591E-5,0.332563288526384));
#15251=CARTESIAN_POINT('',(-0.117821685414254,0.000103165543095151,0.342436711473616));
#15252=CARTESIAN_POINT('',(-0.117775,2.85464118895969E-14,-0.0924367114736175));
#15253=CARTESIAN_POINT('Ctrl Pts',(-0.117911328466355,-7.22474488887752E-5,
0.332563288526384));
#15254=CARTESIAN_POINT('Ctrl Pts',(-0.117942332027964,-0.00437115939612809,
0.332854713939869));
#15255=CARTESIAN_POINT('Ctrl Pts',(-0.115777752883067,-0.0476754067323583,
0.335792469232457));
#15256=CARTESIAN_POINT('Ctrl Pts',(-0.0622106591311991,-0.12453304658572,
0.341376554404146));
#15257=CARTESIAN_POINT('Ctrl Pts',(0.0708961914151981,-0.119801401679107,
0.349315544041452));
#15258=CARTESIAN_POINT('Ctrl Pts',(0.1391024375543,-0.00539978406154301,
0.357254533678757));
#15259=CARTESIAN_POINT('Ctrl Pts',(0.0799699354250877,0.113944965792994,
0.365193523316063));
#15260=CARTESIAN_POINT('Ctrl Pts',(-0.0523695618881846,0.128980908622551,
0.373132512953369));
#15261=CARTESIAN_POINT('Ctrl Pts',(-0.113921748517257,0.0538356345748906,
0.378922434690143));
#15262=CARTESIAN_POINT('Ctrl Pts',(-0.117895144954496,0.00745050051778832,
0.382066026547814));
#15263=CARTESIAN_POINT('Ctrl Pts',(-0.117828183671793,0.000101754196006446,
0.382563288526384));
#15264=CARTESIAN_POINT('Ctrl Pts',(-0.117821685414254,0.000103165543095145,
0.342436711473616));
#15265=CARTESIAN_POINT('Ctrl Pts',(-0.117532262555972,-0.0314544122979593,
0.344571790884339));
#15266=CARTESIAN_POINT('Ctrl Pts',(-0.0882170202347594,-0.102616110661261,
0.349354259669323));
#15267=CARTESIAN_POINT('Ctrl Pts',(0.0320320385160992,-0.135491055083419,
0.356784117828566));
#15268=CARTESIAN_POINT('Ctrl Pts',(0.131227975626944,-0.0465090949381858,
0.364726285951346));
#15269=CARTESIAN_POINT('Ctrl Pts',(0.110205605501345,0.0850799742312894,
0.372668454074126));
#15270=CARTESIAN_POINT('Ctrl Pts',(-0.0117764211155082,0.138727046407055,
0.380610622196906));
#15271=CARTESIAN_POINT('Ctrl Pts',(-0.10403099481448,0.0777947493501838,
0.387200041330069));
#15272=CARTESIAN_POINT('Ctrl Pts',(-0.117591991327853,0.019241607989002,
0.391142071088973));
#15273=CARTESIAN_POINT('Ctrl Pts',(-0.117581664177921,7.09484545444172E-6,
0.392436711473616));
#15274=CARTESIAN_POINT('Origin',(0.,0.,-0.0924367114736175));
#15275=CARTESIAN_POINT('',(-0.117608153246896,-5.64262068778628E-5,0.282563288526383));
#15276=CARTESIAN_POINT('',(-0.117918861549493,-6.80329776671096E-5,0.292436711473615));
#15277=CARTESIAN_POINT('',(-0.117775,2.85464118895969E-14,-0.0924367114736175));
#15278=CARTESIAN_POINT('Ctrl Pts',(-0.117608153246896,-5.64262068778604E-5,
0.282563288526383));
#15279=CARTESIAN_POINT('Ctrl Pts',(-0.117677606263852,-0.0160946837114709,
0.283643401331924));
#15280=CARTESIAN_POINT('Ctrl Pts',(-0.107144424846824,-0.0713401098021974,
0.287369844016567));
#15281=CARTESIAN_POINT('Ctrl Pts',(-0.0229969941138309,-0.137294515779738,
0.293742616580312));
#15282=CARTESIAN_POINT('Ctrl Pts',(0.102883268653204,-0.0937746172089793,
0.301681606217617));
#15283=CARTESIAN_POINT('Ctrl Pts',(0.134580950019115,0.0355895166223291,
0.309620595854923));
#15284=CARTESIAN_POINT('Ctrl Pts',(0.0430789950773988,0.13237388709478,
0.317559585492229));
#15285=CARTESIAN_POINT('Ctrl Pts',(-0.0830523456774332,0.10887452531409,
0.325207149716049));
#15286=CARTESIAN_POINT('Ctrl Pts',(-0.11766079978112,0.0346657214219864,
0.330208384060767));
#15287=CARTESIAN_POINT('Ctrl Pts',(-0.117911328466355,-7.22474488887752E-5,
0.332563288526384));
#15288=CARTESIAN_POINT('Ctrl Pts',(-0.117918861549493,-6.80329776671157E-5,
0.292436711473616));
#15289=CARTESIAN_POINT('Ctrl Pts',(-0.117946256357307,-0.00405052459867665,
0.292706731931186));
#15290=CARTESIAN_POINT('Ctrl Pts',(-0.11595553950755,-0.0470512577090033,
0.295624141763016));
#15291=CARTESIAN_POINT('Ctrl Pts',(-0.0631725212350128,-0.124068972994571,
0.301188940969106));
#15292=CARTESIAN_POINT('Ctrl Pts',(0.0700327441786229,-0.12032993078169,
0.309131109091886));
#15293=CARTESIAN_POINT('Ctrl Pts',(0.139080821187468,-0.00635631000930847,
0.317073277214666));
#15294=CARTESIAN_POINT('Ctrl Pts',(0.0807165776729536,0.11344034374014,
0.325015445337446));
#15295=CARTESIAN_POINT('Ctrl Pts',(-0.0515923433190751,0.129313988454311,
0.332957613460226));
#15296=CARTESIAN_POINT('Ctrl Pts',(-0.113774867115171,0.0543021652640841,
0.338764702172283));
#15297=CARTESIAN_POINT('Ctrl Pts',(-0.117891132111753,0.00767537174388221,
0.341924401510079));
#15298=CARTESIAN_POINT('Ctrl Pts',(-0.117821685414254,0.000103165543095145,
0.342436711473616));
#15299=CARTESIAN_POINT('Origin',(0.,0.,-0.0924367114736175));
#15300=CARTESIAN_POINT('',(-0.117705188630573,0.000102098618198066,0.232563288526383));
#15301=CARTESIAN_POINT('',(-0.1176142238744,-6.23262858038681E-5,0.242436711473616));
#15302=CARTESIAN_POINT('',(-0.117775,2.85464118895969E-14,-0.0924367114736175));
#15303=CARTESIAN_POINT('Ctrl Pts',(-0.117705188630573,0.000102098618198071,
0.232563288526383));
#15304=CARTESIAN_POINT('Ctrl Pts',(-0.117475649963863,-0.0275896003179174,
0.234432088723979));
#15305=CARTESIAN_POINT('Ctrl Pts',(-0.0938913217252411,-0.0948462909608301,
0.238947218800678));
#15306=CARTESIAN_POINT('Ctrl Pts',(0.0182347644767634,-0.138007750384372,
0.246108678756477));
#15307=CARTESIAN_POINT('Ctrl Pts',(0.125841858853055,-0.0595186723796334,
0.254047668393783));
#15308=CARTESIAN_POINT('Ctrl Pts',(0.118249355954961,0.073455671106145,
0.261986658031089));
#15309=CARTESIAN_POINT('Ctrl Pts',(0.00240767183786234,0.139186381940956,
0.269925647668394));
#15310=CARTESIAN_POINT('Ctrl Pts',(-0.0995777503027144,0.0858938305448248,
0.27678452450016));
#15311=CARTESIAN_POINT('Ctrl Pts',(-0.117507442931816,0.0231998416616275,
0.280997071452822));
#15312=CARTESIAN_POINT('Ctrl Pts',(-0.117608153246896,-5.64262068778604E-5,
0.282563288526383));
#15313=CARTESIAN_POINT('Ctrl Pts',(-0.1176142238744,-6.2326285803882E-5,
0.242436711473616));
#15314=CARTESIAN_POINT('Ctrl Pts',(-0.117689148257971,-0.0156863246439697,
0.243489062352292));
#15315=CARTESIAN_POINT('Ctrl Pts',(-0.107519643382358,-0.0705218816827611,
0.247188802605229));
#15316=CARTESIAN_POINT('Ctrl Pts',(-0.024381182195918,-0.137074561658528,
0.253535932232426));
#15317=CARTESIAN_POINT('Ctrl Pts',(0.101985705091022,-0.094777599970642,
0.261478100355206));
#15318=CARTESIAN_POINT('Ctrl Pts',(0.134923209124943,0.0343453801629359,
0.269420268477986));
#15319=CARTESIAN_POINT('Ctrl Pts',(0.0442571924125319,0.132004463632409,
0.277362436600766));
#15320=CARTESIAN_POINT('Ctrl Pts',(-0.0824920331482911,0.109525057495754,
0.285034584265976));
#15321=CARTESIAN_POINT('Ctrl Pts',(-0.117677666622401,0.0349954280503056,
0.290059342556926));
#15322=CARTESIAN_POINT('Ctrl Pts',(-0.117918861549493,-6.80329776671157E-5,
0.292436711473616));
#15323=CARTESIAN_POINT('Origin',(0.,0.,-0.0924367114736175));
#15324=CARTESIAN_POINT('',(-0.117967994073432,-3.0724305424694E-6,0.182563288526383));
#15325=CARTESIAN_POINT('',(-0.117691121003631,9.91971943564221E-5,0.192436711473615));
#15326=CARTESIAN_POINT('',(-0.117775,2.85464118895969E-14,-0.0924367114736175));
#15327=CARTESIAN_POINT('Ctrl Pts',(-0.117967994073432,-3.07243054247449E-6,
0.182563288526383));
#15328=CARTESIAN_POINT('Ctrl Pts',(-0.117968057042159,-0.000167453844217198,
0.182574446236933));
#15329=CARTESIAN_POINT('Ctrl Pts',(-0.117893299674953,-0.0393189363008842,
0.185231933826584));
#15330=CARTESIAN_POINT('Ctrl Pts',(-0.0749972298318695,-0.11727771015962,
0.190535751295337));
#15331=CARTESIAN_POINT('Ctrl Pts',(0.0578663373665801,-0.126610160769685,
0.198474740932643));
#15332=CARTESIAN_POINT('Ctrl Pts',(0.13775723856723,-0.0200396862227523,
0.206413730569949));
#15333=CARTESIAN_POINT('Ctrl Pts',(0.091540828968026,0.104875747581476,
0.214352720207254));
#15334=CARTESIAN_POINT('Ctrl Pts',(-0.0384749358425138,0.133784622116252,
0.22229170984456));
#15335=CARTESIAN_POINT('Ctrl Pts',(-0.110955338697302,0.0622468391270206,
0.22836189928427));
#15336=CARTESIAN_POINT('Ctrl Pts',(-0.11780069007939,0.0116234575531164,
0.231785758844877));
#15337=CARTESIAN_POINT('Ctrl Pts',(-0.117705188630573,0.000102098618198071,
0.232563288526383));
#15338=CARTESIAN_POINT('Ctrl Pts',(-0.117691121003631,9.91971943564221E-5,
0.192436711473615));
#15339=CARTESIAN_POINT('Ctrl Pts',(-0.117474218986382,-0.0270951350261672,
0.194271392773399));
#15340=CARTESIAN_POINT('Ctrl Pts',(-0.0945676524372527,-0.0938598508209937,
0.198753463447442));
#15341=CARTESIAN_POINT('Ctrl Pts',(0.0165156171993534,-0.138242945169174,
0.205882923495746));
#15342=CARTESIAN_POINT('Ctrl Pts',(0.125131592687617,-0.061040658666823,
0.213825091618526));
#15343=CARTESIAN_POINT('Ctrl Pts',(0.119114174013628,0.0720811421096423,
0.221767259741306));
#15344=CARTESIAN_POINT('Ctrl Pts',(0.0039759348809324,0.139169211541763,
0.229709427864086));
#15345=CARTESIAN_POINT('Ctrl Pts',(-0.0990660356104632,0.0867677816679632,
0.236599245108189));
#15346=CARTESIAN_POINT('Ctrl Pts',(-0.117500661679058,0.0236188235484957,
0.240841672978032));
#15347=CARTESIAN_POINT('Ctrl Pts',(-0.1176142238744,-6.2326285803882E-5,
0.242436711473616));
#15348=CARTESIAN_POINT('Origin',(0.,0.,-0.0924367114736175));
#15349=CARTESIAN_POINT('',(-0.117696212882312,-0.000100181105204699,0.132563288526383));
#15350=CARTESIAN_POINT('',(-0.117967699956222,8.3697257429456E-6,0.142436711473616));
#15351=CARTESIAN_POINT('',(-0.117775,2.85464118895969E-14,-0.0924367114736175));
#15352=CARTESIAN_POINT('Ctrl Pts',(-0.117696212882312,-0.000100181105204706,
0.132563288526383));
#15353=CARTESIAN_POINT('Ctrl Pts',(-0.117792074781153,-0.0119544960022407,
0.133363133628988));
#15354=CARTESIAN_POINT('Ctrl Pts',(-0.110696412003459,-0.0629173266909915,
0.136809308610694));
#15355=CARTESIAN_POINT('Ctrl Pts',(-0.0373480950846616,-0.134103559412242,
0.142901813471503));
#15356=CARTESIAN_POINT('Ctrl Pts',(0.0924198687735613,-0.104101940294199,
0.150840803108809));
#15357=CARTESIAN_POINT('Ctrl Pts',(0.137583777756591,0.0211978768359354,
0.158779792746114));
#15358=CARTESIAN_POINT('Ctrl Pts',(0.0567991668878991,0.127092487218924,
0.16671878238342));
#15359=CARTESIAN_POINT('Ctrl Pts',(-0.0757945745091616,0.116657324056303,
0.174646614310176));
#15360=CARTESIAN_POINT('Ctrl Pts',(-0.117953122434976,0.0388197061692436,
0.179928116357831));
#15361=CARTESIAN_POINT('Ctrl Pts',(-0.117967994073432,-3.07243054247449E-6,
0.182563288526383));
#15362=CARTESIAN_POINT('Ctrl Pts',(-0.117967699956222,8.3697257429579E-6,
0.142436711473616));
#15363=CARTESIAN_POINT('Ctrl Pts',(-0.117928252023989,-0.038547130539091,
0.145053723194506));
#15364=CARTESIAN_POINT('Ctrl Pts',(-0.0762804946418446,-0.116178754198862,
0.150318124289656));
#15365=CARTESIAN_POINT('Ctrl Pts',(0.0559861945572589,-0.127473226882309,
0.158229914759066));
#15366=CARTESIAN_POINT('Ctrl Pts',(0.137471621702818,-0.0220324926503626,
0.166172082881846));
#15367=CARTESIAN_POINT('Ctrl Pts',(0.0930189202108026,0.103592267873211,
0.174114251004626));
#15368=CARTESIAN_POINT('Ctrl Pts',(-0.0366486683060043,0.134315868829211,
0.182056419127406));
#15369=CARTESIAN_POINT('Ctrl Pts',(-0.110544190454925,0.0633195416932908,
0.188163905950403));
#15370=CARTESIAN_POINT('Ctrl Pts',(-0.11778720200735,0.0121454601492482,
0.191624003399139));
#15371=CARTESIAN_POINT('Ctrl Pts',(-0.117691121003631,9.91971943564221E-5,
0.192436711473615));
#15372=CARTESIAN_POINT('Origin',(0.,0.,-0.0924367114736175));
#15373=CARTESIAN_POINT('',(-0.117613109409711,6.11591708146705E-5,0.0825632885263832));
#15374=CARTESIAN_POINT('',(-0.117715749944134,-0.000104199409386274,0.0924367114736155));
#15375=CARTESIAN_POINT('',(-0.117775,2.85464118895969E-14,-0.0924367114736175));
#15376=CARTESIAN_POINT('Ctrl Pts',(-0.117613109409711,6.11591708146765E-5,
0.0825632885263832));
#15377=CARTESIAN_POINT('Ctrl Pts',(-0.117502393620717,-0.0235240259785673,
0.0841518210210431));
#15378=CARTESIAN_POINT('Ctrl Pts',(-0.0991849320095013,-0.0865581493706475,
0.088386683394805));
#15379=CARTESIAN_POINT('Ctrl Pts',(0.00357853460314598,-0.139161043603659,
0.0952678756476685));
#15380=CARTESIAN_POINT('Ctrl Pts',(0.118863112008681,-0.0724583686054966,
0.103206865284975));
#15381=CARTESIAN_POINT('Ctrl Pts',(0.125336705278751,0.0605752693714656,
0.11114585492228));
#15382=CARTESIAN_POINT('Ctrl Pts',(0.0170731091066207,0.138156245709763,
0.119084844559586));
#15383=CARTESIAN_POINT('Ctrl Pts',(-0.094337657277608,0.0941904991302726,
0.126223989094287));
#15384=CARTESIAN_POINT('Ctrl Pts',(-0.11747491061231,0.0272661325996615,
0.130716803749886));
#15385=CARTESIAN_POINT('Ctrl Pts',(-0.117696212882312,-0.000100181105204706,
0.132563288526383));
#15386=CARTESIAN_POINT('Ctrl Pts',(-0.117715749944134,-0.000104199409386274,
0.0924367114736155));
#15387=CARTESIAN_POINT('Ctrl Pts',(-0.117810584636384,-0.011244028442556,
0.0931886642413524));
#15388=CARTESIAN_POINT('Ctrl Pts',(-0.111246641208053,-0.0614941526881817,
0.0965880063833492));
#15389=CARTESIAN_POINT('Ctrl Pts',(-0.0397151780004399,-0.133441281507892,
0.102634737899606));
#15390=CARTESIAN_POINT('Ctrl Pts',(0.0906220264938673,-0.105695447092796,
0.110576906022386));
#15391=CARTESIAN_POINT('Ctrl Pts',(0.137940159127448,0.0188783162799928,
0.118519074145166));
#15392=CARTESIAN_POINT('Ctrl Pts',(0.0588909273047484,0.126157580947307,
0.126461242267946));
#15393=CARTESIAN_POINT('Ctrl Pts',(-0.074108440039672,0.117863552156501,
0.134403410390726));
#15394=CARTESIAN_POINT('Ctrl Pts',(-0.117763087033452,0.0399060678969832,
0.139728566792616));
#15395=CARTESIAN_POINT('Ctrl Pts',(-0.117968157858494,0.000455912857932787,
0.142406333820246));
#15396=CARTESIAN_POINT('Ctrl Pts',(-0.117967699956222,8.3697257429579E-6,
0.142436711473616));
#15397=CARTESIAN_POINT('Origin',(0.,0.,-0.0924367114736175));
#15398=CARTESIAN_POINT('',(-0.117917485785546,7.60014832213593E-5,0.0325632885263832));
#15399=CARTESIAN_POINT('',(-0.117600989619072,5.04992496179954E-5,0.0424367114736154));
#15400=CARTESIAN_POINT('',(-0.117775,2.85464118895969E-14,-0.0924367114736175));
#15401=CARTESIAN_POINT('Ctrl Pts',(-0.117917485785546,7.60014832213644E-5,
0.0325632885263832));
#15402=CARTESIAN_POINT('Ctrl Pts',(-0.117676727567847,-0.0349830640657269,
0.0349405084130983));
#15403=CARTESIAN_POINT('Ctrl Pts',(-0.0825043195215805,-0.109517225708346,
0.0399640581789154));
#15404=CARTESIAN_POINT('Ctrl Pts',(0.0441923146003338,-0.131999388615902,
0.0476339378238343));
#15405=CARTESIAN_POINT('Ctrl Pts',(0.134874939024977,-0.034459980695041,
0.0555729274611401));
#15406=CARTESIAN_POINT('Ctrl Pts',(0.102091080224759,0.094638871230671,
0.0635119170984456));
#15407=CARTESIAN_POINT('Ctrl Pts',(-0.0241513666277066,0.137095110112719,
0.0714509067357516));
#15408=CARTESIAN_POINT('Ctrl Pts',(-0.107448046275642,0.0706698818446754,
0.0778013638783972));
#15409=CARTESIAN_POINT('Ctrl Pts',(-0.117686834607281,0.0157664388843013,
0.0815054911419412));
#15410=CARTESIAN_POINT('Ctrl Pts',(-0.117613109409711,6.11591708146765E-5,
0.0825632885263832));
#15411=CARTESIAN_POINT('Ctrl Pts',(-0.117600989619072,5.04992496179954E-5,
0.0424367114736154));
#15412=CARTESIAN_POINT('Ctrl Pts',(-0.117514779739531,-0.0227353060542692,
0.043970994662459));
#15413=CARTESIAN_POINT('Ctrl Pts',(-0.100129952091853,-0.0849605109884783,
0.0481526672255625));
#15414=CARTESIAN_POINT('Ctrl Pts',(0.000787973702835166,-0.139222729671589,
0.054981729162926));
#15415=CARTESIAN_POINT('Ctrl Pts',(0.117431922513572,-0.0747907597173192,
0.0629238972857061));
#15416=CARTESIAN_POINT('Ctrl Pts',(0.126496838785129,0.0581591461343325,
0.070866065408486));
#15417=CARTESIAN_POINT('Ctrl Pts',(0.0196773008918215,0.137828289815661,
0.0788082335312661));
#15418=CARTESIAN_POINT('Ctrl Pts',(-0.0933482651079043,0.0956446566614129,
0.085998448886309));
#15419=CARTESIAN_POINT('Ctrl Pts',(-0.11747670148927,0.0279758085988667,
0.0905412748670923));
#15420=CARTESIAN_POINT('Ctrl Pts',(-0.117715749944134,-0.000104199409386274,
0.0924367114736155));
#15421=CARTESIAN_POINT('Origin',(0.,0.,1.55));
#15422=CARTESIAN_POINT('',(-0.143211704627722,-5.70397197726547E-6,1.50700023576178));
#15423=CARTESIAN_POINT('Ctrl Pts',(-0.0334019664626774,0.112939183906323,
1.532225));
#15424=CARTESIAN_POINT('Ctrl Pts',(-0.0250606930336426,0.115799676338094,
1.53184761307169));
#15425=CARTESIAN_POINT('Ctrl Pts',(-0.0164287086124659,0.117635554524944,
1.53147359869818));
#15426=CARTESIAN_POINT('Ctrl Pts',(-0.00767226928320402,0.118510614220874,
1.53110056493424));
#15427=CARTESIAN_POINT('Ctrl Pts',(-0.0042150196872779,0.118856108509867,
1.53095328237096));
#15428=CARTESIAN_POINT('Ctrl Pts',(-0.000736351480830917,0.119051293525916,
1.53080607672538));
#15429=CARTESIAN_POINT('Ctrl Pts',(0.00274830211697625,0.119097943881266,
1.53065904037218));
#15430=CARTESIAN_POINT('Ctrl Pts',(0.00972321854123044,0.119191319684798,
1.53036473098213));
#15431=CARTESIAN_POINT('Ctrl Pts',(0.0166907125456733,0.118690968429664,
1.53007241075126));
#15432=CARTESIAN_POINT('Ctrl Pts',(0.0235721318645625,0.11762150546261,
1.52978094357425));
#15433=CARTESIAN_POINT('Ctrl Pts',(0.0273478463565568,0.117034709826966,
1.52962102062912));
#15434=CARTESIAN_POINT('Ctrl Pts',(0.0310977188904398,0.116276259986281,
1.52946135449799));
#15435=CARTESIAN_POINT('Ctrl Pts',(0.0348087249896146,0.115347945392283,
1.52930175751644));
#15436=CARTESIAN_POINT('Ctrl Pts',(0.0378768737129624,0.114580442682688,
1.52916980751093));
#15437=CARTESIAN_POINT('Ctrl Pts',(0.0409182562642153,0.113696477767379,
1.52903790896105));
#15438=CARTESIAN_POINT('Ctrl Pts',(0.0439120268522727,0.112701821307647,
1.52890655030309));
#15439=CARTESIAN_POINT('Ctrl Pts',(0.0504861734289241,0.110517613410832,
1.52861809430882));
#15440=CARTESIAN_POINT('Ctrl Pts',(0.0568477403450367,0.107796947733889,
1.528331525126));
#15441=CARTESIAN_POINT('Ctrl Pts',(0.0629211062797432,0.10455513280498,
1.52804576869741));
#15442=CARTESIAN_POINT('Ctrl Pts',(0.0667529140263229,0.102509807084265,
1.52786547926507));
#15443=CARTESIAN_POINT('Ctrl Pts',(0.0704699809867569,0.100256700264741,
1.52768551335768));
#15444=CARTESIAN_POINT('Ctrl Pts',(0.0740519796445933,0.0977963961590643,
1.52750560123222));
#15445=CARTESIAN_POINT('Ctrl Pts',(0.0761474027326905,0.0963571499395001,
1.52740035495562));
#15446=CARTESIAN_POINT('Ctrl Pts',(0.0781972522873126,0.0948464165467323,
1.52729509152825));
#15447=CARTESIAN_POINT('Ctrl Pts',(0.0801950758490376,0.0932655888959708,
1.52718986717129));
#15448=CARTESIAN_POINT('Ctrl Pts',(0.0872135629190184,0.0877120362002772,
1.52682020700562));
#15449=CARTESIAN_POINT('Ctrl Pts',(0.0935342345834078,0.0813437113039547,
1.52645409167081));
#15450=CARTESIAN_POINT('Ctrl Pts',(0.0991216768718319,0.0743433873765979,
1.52608928877518));
#15451=CARTESIAN_POINT('Ctrl Pts',(0.101857856375295,0.0709153174549959,
1.52591064420861));
#15452=CARTESIAN_POINT('Ctrl Pts',(0.104417791592617,0.0673349702414553,
1.52573231437502));
#15453=CARTESIAN_POINT('Ctrl Pts',(0.106794530290299,0.0636205708890664,
1.52555403711528));
#15454=CARTESIAN_POINT('Ctrl Pts',(0.108394385735532,0.0611202951812291,
1.52543403324399));
#15455=CARTESIAN_POINT('Ctrl Pts',(0.109912312880749,0.0585571637778213,
1.52531395827658));
#15456=CARTESIAN_POINT('Ctrl Pts',(0.111341951189028,0.0559432008961949,
1.5251940432238));
#15457=CARTESIAN_POINT('Ctrl Pts',(0.115894033640165,0.0476201345006791,
1.52481222412716));
#15458=CARTESIAN_POINT('Ctrl Pts',(0.119530893641226,0.0388304356906876,
1.52443409356659));
#15459=CARTESIAN_POINT('Ctrl Pts',(0.122195159250079,0.0297595052710396,
1.52405718851832));
#15460=CARTESIAN_POINT('Ctrl Pts',(0.123464283518865,0.0254385629829291,
1.52387764960816));
#15461=CARTESIAN_POINT('Ctrl Pts',(0.124512110981915,0.0210533134598664,
1.52369838877875));
#15462=CARTESIAN_POINT('Ctrl Pts',(0.12532867129748,0.0166220814218575,
1.52351913980531));
#15463=CARTESIAN_POINT('Ctrl Pts',(0.126067828800149,0.012610891624201,
1.52335688207487));
#15464=CARTESIAN_POINT('Ctrl Pts',(0.12661735951473,0.00855739899605222,
1.52319445303817));
#15465=CARTESIAN_POINT('Ctrl Pts',(0.126966826155483,0.00450415768051923,
1.52303280899981));
#15466=CARTESIAN_POINT('Ctrl Pts',(0.127602972227412,-0.00287409603749457,
1.52273856283131));
#15467=CARTESIAN_POINT('Ctrl Pts',(0.12758177643555,-0.010267620141741,
1.52244625042084));
#15468=CARTESIAN_POINT('Ctrl Pts',(0.126865581413421,-0.0175939782534482,
1.52215473434257));
#15469=CARTESIAN_POINT('Ctrl Pts',(0.126426462283551,-0.0220859726121444,
1.52197599770985));
#15470=CARTESIAN_POINT('Ctrl Pts',(0.12572570473317,-0.0265528301690258,
1.52179756043894));
#15471=CARTESIAN_POINT('Ctrl Pts',(0.124776542651163,-0.0309793260681717,
1.52161916036391));
#15472=CARTESIAN_POINT('Ctrl Pts',(0.124151644840291,-0.0338935887106027,
1.52150170748789));
#15473=CARTESIAN_POINT('Ctrl Pts',(0.123418330834614,-0.0367926408403149,
1.52138417707714));
#15474=CARTESIAN_POINT('Ctrl Pts',(0.122581975874549,-0.0396644408336013,
1.52126680258073));
#15475=CARTESIAN_POINT('Ctrl Pts',(0.120074191833131,-0.0482754427851461,
1.52091485884509));
#15476=CARTESIAN_POINT('Ctrl Pts',(0.116656903439717,-0.0566007293654626,
1.52056600333313));
#15477=CARTESIAN_POINT('Ctrl Pts',(0.112443760417108,-0.0645262187619275,
1.52021830866717));
#15478=CARTESIAN_POINT('Ctrl Pts',(0.109356904590302,-0.0703330102694749,
1.51996356219884));
#15479=CARTESIAN_POINT('Ctrl Pts',(0.105841781173658,-0.0759253337267248,
1.51970943888381));
#15480=CARTESIAN_POINT('Ctrl Pts',(0.101930367117466,-0.0812537151913617,
1.51945518067311));
#15481=CARTESIAN_POINT('Ctrl Pts',(0.100130771446666,-0.0837052409256295,
1.51933819945644));
#15482=CARTESIAN_POINT('Ctrl Pts',(0.0982476276828181,-0.0860996963839449,
1.51922123442864));
#15483=CARTESIAN_POINT('Ctrl Pts',(0.0962924325256194,-0.0884227179472683,
1.51910469697823));
#15484=CARTESIAN_POINT('Ctrl Pts',(0.0906946176521128,-0.0950736369671782,
1.51877104482549));
#15485=CARTESIAN_POINT('Ctrl Pts',(0.0844921899154374,-0.101162815315101,
1.51843983772287));
#15486=CARTESIAN_POINT('Ctrl Pts',(0.0777644521522082,-0.106582693579069,
1.51810941878));
#15487=CARTESIAN_POINT('Ctrl Pts',(0.0731067700043679,-0.110334931124879,
1.5178806663426));
#15488=CARTESIAN_POINT('Ctrl Pts',(0.0681966627772886,-0.113766151308436,
1.51765229166508));
#15489=CARTESIAN_POINT('Ctrl Pts',(0.0630541948599911,-0.116833686038022,
1.5174237449583));
#15490=CARTESIAN_POINT('Ctrl Pts',(0.0607686815400033,-0.118197018118406,
1.51732216988754));
#15491=CARTESIAN_POINT('Ctrl Pts',(0.0584414404741937,-0.119485783651375,
1.51722075040181));
#15492=CARTESIAN_POINT('Ctrl Pts',(0.0560784264268894,-0.12069488199044,
1.51711960151386));
#15493=CARTESIAN_POINT('Ctrl Pts',(0.0475595529450054,-0.125053787850271,
1.51675495087613));
#15494=CARTESIAN_POINT('Ctrl Pts',(0.038563113830939,-0.128389854466075,
1.51639315730301));
#15495=CARTESIAN_POINT('Ctrl Pts',(0.0292711048986314,-0.130741856378471,
1.51603205677802));
#15496=CARTESIAN_POINT('Ctrl Pts',(0.0254547302664753,-0.13170786066222,
1.51588374709674));
#15497=CARTESIAN_POINT('Ctrl Pts',(0.0215881861914954,-0.132507324978224,
1.51573555432397));
#15498=CARTESIAN_POINT('Ctrl Pts',(0.0176832233642019,-0.13314066674995,
1.51558732853105));
#15499=CARTESIAN_POINT('Ctrl Pts',(0.0144414794405867,-0.133666441752394,
1.51546427740745));
#15500=CARTESIAN_POINT('Ctrl Pts',(0.0111713231872828,-0.134077605234841,
1.5153411329761));
#15501=CARTESIAN_POINT('Ctrl Pts',(0.00789687394913892,-0.134372952697723,
1.51521845803943));
#15502=CARTESIAN_POINT('Ctrl Pts',(-0.00208492598009478,-0.135273287095873,
1.51484449692866));
#15503=CARTESIAN_POINT('Ctrl Pts',(-0.0121386692885745,-0.135107999768821,
1.51447364169918));
#15504=CARTESIAN_POINT('Ctrl Pts',(-0.0220717676774029,-0.133899092645375,
1.51410356562093));
#15505=CARTESIAN_POINT('Ctrl Pts',(-0.0271373055616968,-0.133282591671289,
1.51391483957382));
#15506=CARTESIAN_POINT('Ctrl Pts',(-0.0321716696217597,-0.132393849601707,
1.51372631615657));
#15507=CARTESIAN_POINT('Ctrl Pts',(-0.0371491047637803,-0.131230566976147,
1.51353768678866));
#15508=CARTESIAN_POINT('Ctrl Pts',(-0.0401763453142056,-0.130523066780721,
1.51342296375255));
#15509=CARTESIAN_POINT('Ctrl Pts',(-0.0431793745847511,-0.129714439573166,
1.51330831773957));
#15510=CARTESIAN_POINT('Ctrl Pts',(-0.0461427198170546,-0.128807808452418,
1.51319405707679));
#15511=CARTESIAN_POINT('Ctrl Pts',(-0.0557912886485991,-0.125855842991896,
1.51282202756853));
#15512=CARTESIAN_POINT('Ctrl Pts',(-0.0650506639775802,-0.121862017750276,
1.51245293010828));
#15513=CARTESIAN_POINT('Ctrl Pts',(-0.0737251756215706,-0.116823260910032,
1.51208446868514));
#15514=CARTESIAN_POINT('Ctrl Pts',(-0.0774533877539874,-0.114657657224767,
1.51192610791459));
#15515=CARTESIAN_POINT('Ctrl Pts',(-0.0810733781510443,-0.112298364258586,
1.51176786463208));
#15516=CARTESIAN_POINT('Ctrl Pts',(-0.0845783705992567,-0.109758519633299,
1.51160955655689));
#15517=CARTESIAN_POINT('Ctrl Pts',(-0.0871260289206952,-0.107912394030924,
1.51149448786814));
#15518=CARTESIAN_POINT('Ctrl Pts',(-0.0896122610481647,-0.105970921032248,
1.51137940572563));
#15519=CARTESIAN_POINT('Ctrl Pts',(-0.0920243025666997,-0.10394826075131,
1.51126473391974));
#15520=CARTESIAN_POINT('Ctrl Pts',(-0.0995315444015674,-0.0976529296958118,
1.51090782920982));
#15521=CARTESIAN_POINT('Ctrl Pts',(-0.106349817996106,-0.090554906599088,
1.51055366538392));
#15522=CARTESIAN_POINT('Ctrl Pts',(-0.112409916721278,-0.0828189535999138,
1.51020021897155));
#15523=CARTESIAN_POINT('Ctrl Pts',(-0.11567060314877,-0.0786565598680515,
1.51001004419521));
#15524=CARTESIAN_POINT('Ctrl Pts',(-0.118711357121208,-0.0743087544864998,
1.50982007711492));
#15525=CARTESIAN_POINT('Ctrl Pts',(-0.121517490738653,-0.0697974244982526,
1.50963000253165));
#15526=CARTESIAN_POINT('Ctrl Pts',(-0.123184827969132,-0.0671169005197731,
1.50951706477726));
#15527=CARTESIAN_POINT('Ctrl Pts',(-0.124768226583796,-0.064379797453554,
1.50940414472167));
#15528=CARTESIAN_POINT('Ctrl Pts',(-0.12625918933752,-0.0616017405091787,
1.50929161182319));
#15529=CARTESIAN_POINT('Ctrl Pts',(-0.131254477666307,-0.0522942005345653,
1.50891458411209));
#15530=CARTESIAN_POINT('Ctrl Pts',(-0.135235816373665,-0.0424980109473837,
1.50854057440173));
#15531=CARTESIAN_POINT('Ctrl Pts',(-0.138100316247284,-0.0323932585971084,
1.50816719719795));
#15532=CARTESIAN_POINT('Ctrl Pts',(-0.139428601593765,-0.027707625827389,
1.5079940600046));
#15533=CARTESIAN_POINT('Ctrl Pts',(-0.140516076092011,-0.0229552175461711,
1.50782105881478));
#15534=CARTESIAN_POINT('Ctrl Pts',(-0.14134846970832,-0.01815262603916,
1.50764795577689));
#15535=CARTESIAN_POINT('Ctrl Pts',(-0.141840021659925,-0.0153165600461233,
1.5075457335416));
#15536=CARTESIAN_POINT('Ctrl Pts',(-0.142241997144177,-0.0124651428186592,
1.50744355431084));
#15537=CARTESIAN_POINT('Ctrl Pts',(-0.142550993842162,-0.00961078035088443,
1.50734168592779));
#15538=CARTESIAN_POINT('Ctrl Pts',(-0.142847161918882,-0.00687492249914849,
1.50724404681617));
#15539=CARTESIAN_POINT('Ctrl Pts',(-0.143058332724879,-0.00413406598225375,
1.5071466105924));
#15540=CARTESIAN_POINT('Ctrl Pts',(-0.143182669649515,-0.00139134585336764,
1.50704933585643));
#15541=CARTESIAN_POINT('Ctrl Pts',(-0.143203595382121,-0.00092974984559876,
1.50703296465278));
#15542=CARTESIAN_POINT('Ctrl Pts',(-0.143222061023464,-0.000468100854706259,
1.50701659802318));
#15543=CARTESIAN_POINT('Ctrl Pts',(-0.143238079070951,-6.41379011939899E-6,
1.50700023577028));
#15544=CARTESIAN_POINT('',(-0.00156744678985144,0.146109855568756,1.50365));
#15545=CARTESIAN_POINT('Ctrl Pts',(-0.00156962371672063,0.146072546381438,
1.50365));
#15546=CARTESIAN_POINT('Ctrl Pts',(-0.011711474284147,0.144648739717271,
1.50495065132295));
#15547=CARTESIAN_POINT('Ctrl Pts',(-0.0216501921041044,0.142222471223284,
1.50626105010813));
#15548=CARTESIAN_POINT('Ctrl Pts',(-0.0312062965385204,0.138804788898175,
1.50759029209282));
#15549=CARTESIAN_POINT('Ctrl Pts',(-0.0379863325344082,0.136379950477271,
1.50853338648503));
#15550=CARTESIAN_POINT('Ctrl Pts',(-0.0445735484268955,0.133455002060128,
1.5094859663039));
#15551=CARTESIAN_POINT('Ctrl Pts',(-0.0508923708069948,0.130021662144985,
1.51045128011208));
#15552=CARTESIAN_POINT('Ctrl Pts',(-0.053607485163773,0.128546401418451,
1.51086606268101));
#15553=CARTESIAN_POINT('Ctrl Pts',(-0.0562647183424556,0.126981576978965,
1.51128195276517));
#15554=CARTESIAN_POINT('Ctrl Pts',(-0.0588579379029418,0.125328026221608,
1.51169910067666));
#15555=CARTESIAN_POINT('Ctrl Pts',(-0.0624505046767585,0.123037247762191,
1.51227700458785));
#15556=CARTESIAN_POINT('Ctrl Pts',(-0.0659209207101175,0.120575889029892,
1.51285741907924));
#15557=CARTESIAN_POINT('Ctrl Pts',(-0.0692542752175272,0.117943487410649,
1.51344114883776));
#15558=CARTESIAN_POINT('Ctrl Pts',(-0.0735613784355843,0.114542101371374,
1.51419539934302));
#15559=CARTESIAN_POINT('Ctrl Pts',(-0.0776398170223455,0.110855132244726,
1.51495518495604));
#15560=CARTESIAN_POINT('Ctrl Pts',(-0.0814741368103916,0.106911749311875,
1.51572224163114));
#15561=CARTESIAN_POINT('Ctrl Pts',(-0.0845038784997064,0.103795829845314,
1.51632834224744));
#15562=CARTESIAN_POINT('Ctrl Pts',(-0.087381117690253,0.10051973853988,
1.51693898261853));
#15563=CARTESIAN_POINT('Ctrl Pts',(-0.0900959757046659,0.0970973798321736,
1.51755501917095));
#15564=CARTESIAN_POINT('Ctrl Pts',(-0.0920052356275281,0.0946905606587243,
1.51798825505079));
#15565=CARTESIAN_POINT('Ctrl Pts',(-0.093830595110286,0.092215607777745,
1.51842338946406));
#15566=CARTESIAN_POINT('Ctrl Pts',(-0.0955653742165971,0.0896840982544811,
1.51885969689116));
#15567=CARTESIAN_POINT('Ctrl Pts',(-0.0997851775729162,0.0835262696618028,
1.51992100293214));
#15568=CARTESIAN_POINT('Ctrl Pts',(-0.103479134251024,0.0770231540939269,
1.52099120961793));
#15569=CARTESIAN_POINT('Ctrl Pts',(-0.106606394578922,0.0702509006766953,
1.52207541818308));
#15570=CARTESIAN_POINT('Ctrl Pts',(-0.108879606303698,0.0653281362576702,
1.52286353153598));
#15571=CARTESIAN_POINT('Ctrl Pts',(-0.110852991156964,0.0602629640702717,
1.52365904329275));
#15572=CARTESIAN_POINT('Ctrl Pts',(-0.112503888351057,0.0550849881514033,
1.524463912762));
#15573=CARTESIAN_POINT('Ctrl Pts',(-0.113450017754745,0.0521174894567802,
1.52492518356294));
#15574=CARTESIAN_POINT('Ctrl Pts',(-0.114289979676541,0.0491121240008169,
1.52538965304266));
#15575=CARTESIAN_POINT('Ctrl Pts',(-0.115015874151616,0.0460903162170444,
1.52585530945224));
#15576=CARTESIAN_POINT('Ctrl Pts',(-0.117053612444637,0.0376074669234184,
1.52716250482259));
#15577=CARTESIAN_POINT('Ctrl Pts',(-0.118206139871793,0.0289652499882669,
1.52848357355921));
#15578=CARTESIAN_POINT('Ctrl Pts',(-0.11838625730212,0.0202925750432425,
1.52982832573377));
#15579=CARTESIAN_POINT('Ctrl Pts',(-0.118492077855379,0.015197303257165,
1.53061837930521));
#15580=CARTESIAN_POINT('Ctrl Pts',(-0.118261361656021,0.0100916471271278,
1.53141660760476));
#15581=CARTESIAN_POINT('Ctrl Pts',(-0.11766859746431,0.00500517689818842,
1.532225));
#15582=CARTESIAN_POINT('',(-0.115079981391543,0.0902137050004572,1.50365));
#15583=CARTESIAN_POINT('Origin',(0.,0.,1.50365));
#15584=CARTESIAN_POINT('Ctrl Pts',(-0.143238079070951,-6.41379011939899E-6,
1.50700023577028));
#15585=CARTESIAN_POINT('Ctrl Pts',(-0.143514357617001,0.00795674345750163,
1.50671802038504));
#15586=CARTESIAN_POINT('Ctrl Pts',(-0.14306421847979,0.0159310909218757,
1.50643710681857));
#15587=CARTESIAN_POINT('Ctrl Pts',(-0.141940608246003,0.023841490005315,
1.50615648267927));
#15588=CARTESIAN_POINT('Ctrl Pts',(-0.141317731836386,0.0282266413964,1.50600091791928));
#15589=CARTESIAN_POINT('Ctrl Pts',(-0.14048752132733,0.0325921818867556,
1.50584544210227));
#15590=CARTESIAN_POINT('Ctrl Pts',(-0.139456452513291,0.0369250818702156,
1.5056898827608));
#15591=CARTESIAN_POINT('Ctrl Pts',(-0.138790989895207,0.0397215809279161,
1.50558948313156));
#15592=CARTESIAN_POINT('Ctrl Pts',(-0.138042009924554,0.0425029011667524,
1.50548910366784));
#15593=CARTESIAN_POINT('Ctrl Pts',(-0.137214434473447,0.0452564915355094,
1.50538902890071));
#15594=CARTESIAN_POINT('Ctrl Pts',(-0.134176751889031,0.0553637675507716,
1.50502169637912));
#15595=CARTESIAN_POINT('Ctrl Pts',(-0.130076454936343,0.0651325632434767,
1.50465723703036));
#15596=CARTESIAN_POINT('Ctrl Pts',(-0.125018127980614,0.0743940890034878,
1.50429344851366));
#15597=CARTESIAN_POINT('Ctrl Pts',(-0.122034683484208,0.0798566160996726,
1.50407888293545));
#15598=CARTESIAN_POINT('Ctrl Pts',(-0.118716925567465,0.0851425936725427,
1.50386455072235));
#15599=CARTESIAN_POINT('Ctrl Pts',(-0.115078604842436,0.0902138214954005,
1.50365));
#15600=CARTESIAN_POINT('',(-0.05,-6.12323399573677E-18,1.6));
#15601=CARTESIAN_POINT('',(-0.1,-1.22464679914735E-17,1.55));
#15602=CARTESIAN_POINT('Origin',(0.,0.,1.6));
#15603=CARTESIAN_POINT('Ctrl Pts',(0.0850780204044575,-0.11908002747757,
-0.0164977839420936));
#15604=CARTESIAN_POINT('Ctrl Pts',(0.124677800165771,-0.0907875342533835,
-0.0138514540629917));
#15605=CARTESIAN_POINT('Ctrl Pts',(0.172751483861701,0.00791416360185712,
-0.00855879430478784));
#15606=CARTESIAN_POINT('Ctrl Pts',(0.0868617128612901,0.149726167188418,
-0.000619804667482127));
#15607=CARTESIAN_POINT('Ctrl Pts',(-0.078614020905812,0.154028602276276,
0.00731918496982359));
#15608=CARTESIAN_POINT('Ctrl Pts',(-0.172087192378165,0.0175525219725009,
0.0152581746071293));
#15609=CARTESIAN_POINT('Ctrl Pts',(-0.108045720411827,-0.135108484733225,
0.0231971642444351));
#15610=CARTESIAN_POINT('Ctrl Pts',(0.0549144151285058,-0.164025561655164,
0.0311361538817407));
#15611=CARTESIAN_POINT('Ctrl Pts',(0.167598788591005,-0.0428207868793744,
0.0390751435190465));
#15612=CARTESIAN_POINT('Ctrl Pts',(0.126860790413016,0.117600499296196,
0.0470141331563521));
#15613=CARTESIAN_POINT('Ctrl Pts',(-0.0300110592737492,0.170357625684536,
0.054953122793658));
#15614=CARTESIAN_POINT('Ctrl Pts',(-0.159409054995301,0.0671687418111174,
0.0628921124309635));
#15615=CARTESIAN_POINT('Ctrl Pts',(-0.142879399887002,-0.0975110083167992,
0.0708311020682695));
#15616=CARTESIAN_POINT('Ctrl Pts',(0.00444677171871267,-0.172924803493063,
0.078770091705575));
#15617=CARTESIAN_POINT('Ctrl Pts',(0.147702113712341,-0.0900384822365835,
0.0867090813428809));
#15618=CARTESIAN_POINT('Ctrl Pts',(0.155746353789385,0.0752722621313087,
0.0946480709801864));
#15619=CARTESIAN_POINT('Ctrl Pts',(0.021215449100004,0.17167621786987,0.102587060617492));
#15620=CARTESIAN_POINT('Ctrl Pts',(-0.132736728465598,0.110922462699857,
0.110526050254798));
#15621=CARTESIAN_POINT('Ctrl Pts',(-0.165177537004225,-0.0513732581591355,
0.118465039892104));
#15622=CARTESIAN_POINT('Ctrl Pts',(-0.0464096261145344,-0.166640254043574,
0.126404029529409));
#15623=CARTESIAN_POINT('Ctrl Pts',(0.114843114370719,-0.129359532685675,
0.134343019166715));
#15624=CARTESIAN_POINT('Ctrl Pts',(0.170964855654229,0.0263409830179588,
0.142282008804021));
#15625=CARTESIAN_POINT('Ctrl Pts',(0.0705799878925336,0.157928129946847,
0.150220998441327));
#15626=CARTESIAN_POINT('Ctrl Pts',(-0.0944160212638482,0.144942899583874,
0.158159988078632));
#15627=CARTESIAN_POINT('Ctrl Pts',(-0.172980633894512,-0.000727622896455919,
0.166098977715938));
#15628=CARTESIAN_POINT('Ctrl Pts',(-0.0931933312323777,-0.145732055885043,
0.174037967353244));
#15629=CARTESIAN_POINT('Ctrl Pts',(0.0719060791645076,-0.157328779695546,
0.181976956990549));
#15630=CARTESIAN_POINT('Ctrl Pts',(0.171180402159323,-0.0249017879745179,
0.189915946627855));
#15631=CARTESIAN_POINT('Ctrl Pts',(0.113750798721884,0.13032108391891,0.197854936265161));
#15632=CARTESIAN_POINT('Ctrl Pts',(-0.0478098650864174,0.16624393501773,
0.205793925902467));
#15633=CARTESIAN_POINT('Ctrl Pts',(-0.16560387403618,0.0499818570245514,
0.213732915539772));
#15634=CARTESIAN_POINT('Ctrl Pts',(-0.131798885878402,-0.112035185581475,
0.221671905177078));
#15635=CARTESIAN_POINT('Ctrl Pts',(0.0226589495323734,-0.171491694067101,
0.229610894814384));
#15636=CARTESIAN_POINT('Ctrl Pts',(0.156374069566079,-0.073959309724122,
0.237549884451689));
#15637=CARTESIAN_POINT('Ctrl Pts',(0.146939445926624,0.0912777539068999,
0.245488874088995));
#15638=CARTESIAN_POINT('Ctrl Pts',(0.00299182995941577,0.172956289510158,
0.253427863726301));
#15639=CARTESIAN_POINT('Ctrl Pts',(-0.143694601292225,0.0963051955349955,
0.261366853363607));
#15640=CARTESIAN_POINT('Ctrl Pts',(-0.15883847309497,-0.0685067047260848,
0.269305843000912));
#15641=CARTESIAN_POINT('Ctrl Pts',(-0.0285766086907934,-0.170605411881679,
0.277244832638218));
#15642=CARTESIAN_POINT('Ctrl Pts',(0.12784518248692,-0.116526556812001,
0.285183822275524));
#15643=CARTESIAN_POINT('Ctrl Pts',(0.167233470900423,0.0442243749325307,
0.293122811912829));
#15644=CARTESIAN_POINT('Ctrl Pts',(0.0535309779628647,0.164490922320707,
0.301061801550136));
#15645=CARTESIAN_POINT('Ctrl Pts',(-0.109175456582181,0.134177303623408,
0.309000791187441));
#15646=CARTESIAN_POINT('Ctrl Pts',(-0.171939242908932,-0.0189664407699395,
0.316939780824747));
#15647=CARTESIAN_POINT('Ctrl Pts',(-0.0773044361184472,-0.154747708493488,
0.324878770462053));
#15648=CARTESIAN_POINT('Ctrl Pts',(0.0880972839194656,-0.148868054644337,
0.332817760099358));
#15649=CARTESIAN_POINT('Ctrl Pts',(0.172851978230285,-0.00670989936239309,
0.340756749736664));
#15650=CARTESIAN_POINT('Ctrl Pts',(0.0993725327910066,0.141590708926387,
0.34869573937397));
#15651=CARTESIAN_POINT('Ctrl Pts',(-0.0650756559739905,0.160274727038081,
0.356634729011275));
#15652=CARTESIAN_POINT('Ctrl Pts',(-0.169951541620772,0.0322382168908211,
0.364573718648582));
#15653=CARTESIAN_POINT('Ctrl Pts',(-0.119248438453561,-0.125310171390688,
0.372512708285886));
#15654=CARTESIAN_POINT('Ctrl Pts',(0.0406184374886585,-0.168145685830938,
0.380451697923193));
#15655=CARTESIAN_POINT('Ctrl Pts',(0.163301917673335,-0.0570553486694088,
0.388390687560498));
#15656=CARTESIAN_POINT('Ctrl Pts',(0.136493684039406,0.106265249940549,
0.396329677197804));
#15657=CARTESIAN_POINT('Ctrl Pts',(-0.0152651628095069,0.172307295063139,
0.404268666835109));
#15658=CARTESIAN_POINT('Ctrl Pts',(-0.153049799296248,0.0806138205455782,
0.412207656472416));
#15659=CARTESIAN_POINT('Ctrl Pts',(-0.150727833715048,-0.0848760818555219,
0.420146646109721));
#15660=CARTESIAN_POINT('Ctrl Pts',(-0.0104248664208018,-0.172667748255674,
0.428085635747027));
#15661=CARTESIAN_POINT('Ctrl Pts',(0.139421351618932,-0.10239392482138,
0.436024625384332));
#15662=CARTESIAN_POINT('Ctrl Pts',(0.16163687742079,0.0616145192729195,
0.443963615021638));
#15663=CARTESIAN_POINT('Ctrl Pts',(0.0358849196425865,0.169219093691645,
0.451902604658944));
#15664=CARTESIAN_POINT('Ctrl Pts',(-0.122717222714247,0.121915185177559,
0.45984159429625));
#15665=CARTESIAN_POINT('Ctrl Pts',(-0.168980158036723,-0.0369937199732681,
0.467780583933555));
#15666=CARTESIAN_POINT('Ctrl Pts',(-0.0605533396431397,-0.162037409833775,
0.475719573570861));
#15667=CARTESIAN_POINT('Ctrl Pts',(0.103305911202344,-0.138746956140414,
0.483658563208167));
#15668=CARTESIAN_POINT('Ctrl Pts',(0.172595680358559,0.0115568269495825,
0.491597552845473));
#15669=CARTESIAN_POINT('Ctrl Pts',(0.0838859329010004,0.151281127008313,
0.499536542482778));
#15670=CARTESIAN_POINT('Ctrl Pts',(-0.0816156370489812,0.152517923263679,
0.507475532120084));
#15671=CARTESIAN_POINT('Ctrl Pts',(-0.172403684765527,0.0141350135070757,
0.51541452175739));
#15672=CARTESIAN_POINT('Ctrl Pts',(-0.105367974675403,-0.137187532379513,
0.523353511394695));
#15673=CARTESIAN_POINT('Ctrl Pts',(0.0581248948911363,-0.162924294448283,
0.531292501032001));
#15674=CARTESIAN_POINT('Ctrl Pts',(0.168408406744046,-0.039515030880773,
0.539231490669306));
#15675=CARTESIAN_POINT('Ctrl Pts',(0.124525564004667,0.120067535316156,
0.547170480306613));
#15676=CARTESIAN_POINT('Ctrl Pts',(-0.0333518982867267,0.169736501696743,
0.555109469943918));
#15677=CARTESIAN_POINT('Ctrl Pts',(-0.160697983451488,0.0640233335761385,
0.563048459581225));
#15678=CARTESIAN_POINT('Ctrl Pts',(-0.14093607811848,-0.100298808627811,
0.570987449218529));
#15679=CARTESIAN_POINT('Ctrl Pts',(0.00784314775175556,-0.172804265459278,
0.578926438855836));
#15680=CARTESIAN_POINT('Ctrl Pts',(0.149442509381278,-0.0871192603125336,
0.586865428493141));
#15681=CARTESIAN_POINT('Ctrl Pts',(0.154237495636292,0.0783174569774929,
0.594804418130446));
#15682=CARTESIAN_POINT('Ctrl Pts',(0.0178386252221998,0.172059909850489,
0.602743407767753));
#15683=CARTESIAN_POINT('Ctrl Pts',(-0.134890284021987,0.108293307291099,
0.610682397405058));
#15684=CARTESIAN_POINT('Ctrl Pts',(-0.164136382878957,-0.0546083962682395,
0.618621387042364));
#15685=CARTESIAN_POINT('Ctrl Pts',(-0.0431268722112106,-0.167519855601819,
0.62656037667967));
#15686=CARTESIAN_POINT('Ctrl Pts',(0.117362334288317,-0.127078368017432,
0.634499366316975));
#15687=CARTESIAN_POINT('Ctrl Pts',(0.170414367112955,0.0296946562375699,
0.642438355954282));
#15688=CARTESIAN_POINT('Ctrl Pts',(0.0674637261050104,0.159284257814778,
0.650377345591586));
#15689=CARTESIAN_POINT('Ctrl Pts',(-0.0972453325609638,0.143060037825677,
0.658316335228894));
#15690=CARTESIAN_POINT('Ctrl Pts',(-0.172932953925271,-0.00412584224812367,
0.666255324866198));
#15691=CARTESIAN_POINT('Ctrl Pts',(-0.0903123078403481,-0.147534796506203,
0.674194314503505));
#15692=CARTESIAN_POINT('Ctrl Pts',(0.0749830665657334,-0.155885755782802,
0.68213330414081));
#15693=CARTESIAN_POINT('Ctrl Pts',(0.17163658245605,-0.021533989188811,
0.690072293778116));
#15694=CARTESIAN_POINT('Ctrl Pts',(0.11116857013107,0.132530668686874,0.698011283415421));
#15695=CARTESIAN_POINT('Ctrl Pts',(-0.0510666492692211,0.165272582299639,
0.705950273052727));
#15696=CARTESIAN_POINT('Ctrl Pts',(-0.166553851089581,0.0467187736868841,
0.713889262690032));
#15697=CARTESIAN_POINT('Ctrl Pts',(-0.129572416918314,-0.114602870389546,
0.721828252327339));
#15698=CARTESIAN_POINT('Ctrl Pts',(0.0260236847639906,-0.171013440871999,
0.729767241964644));
#15699=CARTESIAN_POINT('Ctrl Pts',(0.157796886564457,-0.0708729265526718,
0.73770623160195));
#15700=CARTESIAN_POINT('Ctrl Pts',(0.145117853242075,0.0941468947867542,
0.745645221239255));
#15701=CARTESIAN_POINT('Ctrl Pts',(-0.000406629147419015,0.172981686256994,
0.753584210876562));
#15702=CARTESIAN_POINT('Ctrl Pts',(-0.145558870420566,0.0934635991681543,
0.761523200513868));
#15703=CARTESIAN_POINT('Ctrl Pts',(-0.157461941624574,-0.0716140074803496,
0.769462190151172));
#15704=CARTESIAN_POINT('Ctrl Pts',(-0.0252193968429213,-0.17113389830906,
0.777401179788479));
#15705=CARTESIAN_POINT('Ctrl Pts',(0.130109777350283,-0.113992433807847,
0.785340169425784));
#15706=CARTESIAN_POINT('Ctrl Pts',(0.166332367384696,0.0475012914327479,
0.793279159063091));
#15707=CARTESIAN_POINT('Ctrl Pts',(0.0502890745800368,0.165510839842773,
0.801218148700395));
#15708=CARTESIAN_POINT('Ctrl Pts',(-0.111790419467279,0.132006557575396,
0.809157138337702));
#15709=CARTESIAN_POINT('Ctrl Pts',(-0.171533445990104,-0.0223406811520247,
0.817096127975007));
#15710=CARTESIAN_POINT('Ctrl Pts',(-0.0742493586638003,-0.156236557391639,
0.825035117612313));
#15711=CARTESIAN_POINT('Ctrl Pts',(0.0910049278783345,-0.147108572929777,
0.832974107249618));
#15712=CARTESIAN_POINT('Ctrl Pts',(0.172950439922886,-0.00331277195964383,
0.840913096886925));
#15713=CARTESIAN_POINT('Ctrl Pts',(0.0965716772857839,0.143515644700454,
0.848852086524229));
#15714=CARTESIAN_POINT('Ctrl Pts',(-0.0682118374171683,0.158965324406771,
0.856791076161536));
#15715=CARTESIAN_POINT('Ctrl Pts',(-0.170552089827228,0.0288931442238776,
0.864730065798841));
#15716=CARTESIAN_POINT('Ctrl Pts',(-0.116763592698541,-0.127628729319482,
0.872669055436147));
#15717=CARTESIAN_POINT('Ctrl Pts',(0.0439139712140358,-0.167315248138923,
0.880608045073453));
#15718=CARTESIAN_POINT('Ctrl Pts',(0.164391304101163,-0.0538361241500125,
0.888547034710759));
#15719=CARTESIAN_POINT('Ctrl Pts',(0.134379664555536,0.108926281867684,
0.896486024348063));
#15720=CARTESIAN_POINT('Ctrl Pts',(-0.018647348250808,0.17197414204115,
0.904425013985371));
#15721=CARTESIAN_POINT('Ctrl Pts',(-0.154603991719776,0.0775914613336281,
0.912364003622676));
#15722=CARTESIAN_POINT('Ctrl Pts',(-0.149031276472826,-0.0878208845346985,
0.920302993259982));
#15723=CARTESIAN_POINT('Ctrl Pts',(-0.00703064139541984,-0.172839229369798,
0.928241982897287));
#15724=CARTESIAN_POINT('Ctrl Pts',(0.141406064038169,-0.099635105162837,
0.936180972534593));
#15725=CARTESIAN_POINT('Ctrl Pts',(0.160395209035295,0.064778129380991,
0.944119962171899));
#15726=CARTESIAN_POINT('Ctrl Pts',(0.03255353276219,0.169891426011666,0.952058951809204));
#15727=CARTESIAN_POINT('Ctrl Pts',(-0.125088671715395,0.119480765548496,
0.959997941446511));
#15728=CARTESIAN_POINT('Ctrl Pts',(-0.168220770124088,-0.040306347222682,
0.967936931083815));
#15729=CARTESIAN_POINT('Ctrl Pts',(-0.0573582824064844,-0.163195761485875,
0.975875920721122));
#15730=CARTESIAN_POINT('Ctrl Pts',(0.106011781834435,-0.136690640644722,
0.983814910358427));
#15731=CARTESIAN_POINT('Ctrl Pts',(0.17233532526783,0.014945393685262,0.991753899995733));
#15732=CARTESIAN_POINT('Ctrl Pts',(0.0808976893297158,0.152899944371113,
0.999692889633039));
#15733=CARTESIAN_POINT('Ctrl Pts',(-0.0845962369090198,0.150885074902754,
1.00763187927034));
#15734=CARTESIAN_POINT('Ctrl Pts',(-0.172648106016301,0.0107452601904448,
1.01557086890765));
#15735=CARTESIAN_POINT('Ctrl Pts',(-0.102652466413112,-0.13923110380544,
1.02350985854496));
#15736=CARTESIAN_POINT('Ctrl Pts',(0.0613144709582997,-0.161750934398167,
1.03144884818226));
#15737=CARTESIAN_POINT('Ctrl Pts',(0.169152212322519,-0.0361988700648799,
1.03938783781957));
#15738=CARTESIAN_POINT('Ctrl Pts',(0.122142696063681,0.12249077894222,1.04732682745687));
#15739=CARTESIAN_POINT('Ctrl Pts',(-0.0366800874558037,0.169048514669047,
1.05526581709418));
#15740=CARTESIAN_POINT('Ctrl Pts',(-0.161924764760067,0.0608539208677085,
1.06320480673148));
#15741=CARTESIAN_POINT('Ctrl Pts',(-0.138938417355371,-0.103048266896446,
1.07114379636879));
#15742=CARTESIAN_POINT('Ctrl Pts',(0.011236529066559,-0.172616828675865,
1.0790827860061));
#15743=CARTESIAN_POINT('Ctrl Pts',(0.151125203217684,-0.0841665140064042,
1.0870217756434));
#15744=CARTESIAN_POINT('Ctrl Pts',(0.152669111109608,0.0813324759279986,
1.09496076528071));
#15745=CARTESIAN_POINT('Ctrl Pts',(0.0144549108781955,0.172377158228925,
1.10289975491801));
#15746=CARTESIAN_POINT('Ctrl Pts',(-0.136991769602464,0.10562236594946,
1.11083874455532));
#15747=CARTESIAN_POINT('Ctrl Pts',(-0.163031873671196,-0.0578224635832477,
1.11877773419263));
#15748=CARTESIAN_POINT('Ctrl Pts',(-0.0398274706979539,-0.168334790537727,
1.12671672382993));
#15749=CARTESIAN_POINT('Ctrl Pts',(0.119836252144435,-0.124748153491552,
1.13465571346724));
#15750=CARTESIAN_POINT('Ctrl Pts',(0.169798099063322,0.0330368685268242,
1.14259470310454));
#15751=CARTESIAN_POINT('Ctrl Pts',(0.0643214233134591,0.160578901573361,
1.15053369274185));
#15752=CARTESIAN_POINT('Ctrl Pts',(-0.100037107244844,0.141121955420339,
1.15847268237915));
#15753=CARTESIAN_POINT('Ctrl Pts',(-0.172818522111203,-0.00752246920075927,
1.16641167201646));
#15754=CARTESIAN_POINT('Ctrl Pts',(-0.0873964240115842,-0.149280588817046,
1.17435066165376));
#15755=CARTESIAN_POINT('Ctrl Pts',(0.0780311106025284,-0.154382560238235,
1.18228965129107));
#15756=CARTESIAN_POINT('Ctrl Pts',(0.172026511281289,-0.01815787828917,
1.19022864092837));
#15757=CARTESIAN_POINT('Ctrl Pts',(0.10854343062882,0.134689096792963,1.19816763056568));
#15758=CARTESIAN_POINT('Ctrl Pts',(-0.0543037217972188,0.164237434607784,
1.20610662020299));
#15759=CARTESIAN_POINT('Ctrl Pts',(-0.167439538594998,0.0434376569656869,
1.21404560984029));
#15760=CARTESIAN_POINT('Ctrl Pts',(-0.127295933190098,-0.117126318651471,
1.2219845994776));
#15761=CARTESIAN_POINT('Ctrl Pts',(0.0293783748903316,-0.170469176734012,
1.2299235891149));
#15762=CARTESIAN_POINT('Ctrl Pts',(0.159158794190081,-0.0677591865323411,
1.23786257875221));
#15763=CARTESIAN_POINT('Ctrl Pts',(0.143240245273553,0.0969796950995427,
1.24580156838952));
#15764=CARTESIAN_POINT('Ctrl Pts',(-0.00380493129617075,0.172940312320012,
1.25374055802682));
#15765=CARTESIAN_POINT('Ctrl Pts',(-0.147366954032488,0.0905859259858403,
1.26167954766413));
#15766=CARTESIAN_POINT('Ctrl Pts',(-0.156024630070406,-0.074693667330688,
1.26961853730143));
#15767=CARTESIAN_POINT('Ctrl Pts',(-0.0218524503424686,-0.171596327294885,
1.27755752693874));
#15768=CARTESIAN_POINT('Ctrl Pts',(0.132324150022753,-0.111414309889572,
1.28549651657604));
#15769=CARTESIAN_POINT('Ctrl Pts',(0.165367059817933,0.0507598725070622,
1.29343550621335));
#15770=CARTESIAN_POINT('Ctrl Pts',(0.0470277596764783,0.166466870408131,
1.30137449585065));
#15771=CARTESIAN_POINT('Ctrl Pts',(-0.114362231391601,0.129784857201791,
1.30931348548797));
#15772=CARTESIAN_POINT('Ctrl Pts',(-0.171061437441431,-0.0257062980954763,
1.31725247512526));
#15773=CARTESIAN_POINT('Ctrl Pts',(-0.071165620995849,-0.157665099140374,
1.32519146476257));
#15774=CARTESIAN_POINT('Ctrl Pts',(0.0938774439379855,-0.145292307632914,
1.33313045439988));
#15775=CARTESIAN_POINT('Ctrl Pts',(0.172982143233999,8.56343898915854E-5,
1.34106944403719));
#15776=CARTESIAN_POINT('Ctrl Pts',(0.0937335447930804,0.145385183220099,
1.34900843367449));
#15777=CARTESIAN_POINT('Ctrl Pts',(-0.0713216883190155,0.157594562185848,
1.3569474233118));
#15778=CARTESIAN_POINT('Ctrl Pts',(-0.171086806821499,0.0255369173285507,
1.3648864129491));
#15779=CARTESIAN_POINT('Ctrl Pts',(-0.114233673229396,-0.129898019862958,
1.37282540258641));
#15780=CARTESIAN_POINT('Ctrl Pts',(0.0471925482590101,-0.166420232464351,
1.38076439222371));
#15781=CARTESIAN_POINT('Ctrl Pts',(0.165417247017141,-0.0505961085897048,
1.38870338186102));
#15782=CARTESIAN_POINT('Ctrl Pts',(0.132213753266125,0.111545248710567,
1.39664237149832));
#15783=CARTESIAN_POINT('Ctrl Pts',(-0.0220222951247444,0.17157464463752,
1.40458136113563));
#15784=CARTESIAN_POINT('Ctrl Pts',(-0.156098584526576,0.0745390809398717,
1.41252035077293));
#15785=CARTESIAN_POINT('Ctrl Pts',(-0.147277046608992,-0.0907316537045687,
1.42045934041024));
#15786=CARTESIAN_POINT('Ctrl Pts',(-0.00363398118293899,-0.172944250658386,
1.42839833004755));
#15787=CARTESIAN_POINT('Ctrl Pts',(0.143336722904634,-0.0968373407211472,
1.43633731968485));
#15788=CARTESIAN_POINT('Ctrl Pts',(0.159090624036536,0.0679158129692223,
1.44427630932216));
#15789=CARTESIAN_POINT('Ctrl Pts',(0.0292114869387437,0.170499931406899,
1.45221529895946));
#15790=CARTESIAN_POINT('Ctrl Pts',(-0.127415456569397,0.116996902323752,
1.46015428859677));
#15791=CARTESIAN_POINT('Ctrl Pts',(-0.167389576437263,-0.0435971050111283,
1.46809327823408));
#15792=CARTESIAN_POINT('Ctrl Pts',(-0.0541541359620402,-0.164303103757731,
1.47603226787138));
#15793=CARTESIAN_POINT('Ctrl Pts',(0.108701533888403,-0.13455879509903,
1.48397125750869));
#15794=CARTESIAN_POINT('Ctrl Pts',(0.171961157005542,0.0182848320604298,
1.49191024714599));
#15795=CARTESIAN_POINT('Ctrl Pts',(0.0779697431325927,0.154543202561513,
1.4998492367833));
#15796=CARTESIAN_POINT('Ctrl Pts',(-0.0877325682749983,0.149025855561406,
1.5077882264206));
#15797=CARTESIAN_POINT('Ctrl Pts',(-0.144149484752264,0.0548439265155397,
1.51308088617881));
#15798=CARTESIAN_POINT('Ctrl Pts',(-0.146217781693078,0.00621955116994065,
1.51572721605791));
#15799=CARTESIAN_POINT('Ctrl Pts',(0.0795408277542855,-0.111329858282327,
-0.0109985226280624));
#15800=CARTESIAN_POINT('Ctrl Pts',(0.116563307192903,-0.0848787452970238,
-0.00835219274896048));
#15801=CARTESIAN_POINT('Ctrl Pts',(0.16150817751539,0.00739908052493189,
-0.00305953299075667));
#15802=CARTESIAN_POINT('Ctrl Pts',(0.0812084309002137,0.139981433724326,
0.00487945664654907));
#15803=CARTESIAN_POINT('Ctrl Pts',(-0.0734975292821143,0.144003850402812,
0.0128184462838548));
#15804=CARTESIAN_POINT('Ctrl Pts',(-0.160887120581772,0.0164101388376342,
0.0207574359211605));
#15805=CARTESIAN_POINT('Ctrl Pts',(-0.101013704785435,-0.126315124179183,
0.0286964255584662));
#15806=CARTESIAN_POINT('Ctrl Pts',(0.0513403816191153,-0.153350170642076,
0.0366354151957719));
#15807=CARTESIAN_POINT('Ctrl Pts',(0.156690838735662,-0.0400338514845966,
0.0445744048330777));
#15808=CARTESIAN_POINT('Ctrl Pts',(0.118604220350264,0.109946623274354,
0.0525133944703833));
#15809=CARTESIAN_POINT('Ctrl Pts',(-0.0280578283917351,0.15927012049393,
0.0604523841076892));
#15810=CARTESIAN_POINT('Ctrl Pts',(-0.14903412333264,0.0627971513379326,
0.0683913737449947));
#15811=CARTESIAN_POINT('Ctrl Pts',(-0.133580279395553,-0.0911646307683348,
0.0763303633823007));
#15812=CARTESIAN_POINT('Ctrl Pts',(0.0041573593468571,-0.161670216863261,
0.0842693530196062));
#15813=CARTESIAN_POINT('Ctrl Pts',(0.138089113144455,-0.0841784443595545,
0.0922083426569122));
#15814=CARTESIAN_POINT('Ctrl Pts',(0.14560980428584,0.0703732645446943,
0.100147332294218));
#15815=CARTESIAN_POINT('Ctrl Pts',(0.0198346691022095,0.160502893816501,
0.108086321931524));
#15816=CARTESIAN_POINT('Ctrl Pts',(-0.124097730593135,0.103703218031488,
0.116025311568829));
#15817=CARTESIAN_POINT('Ctrl Pts',(-0.154427171169137,-0.0480296962598115,
0.123964301206135));
#15818=CARTESIAN_POINT('Ctrl Pts',(-0.0433891157712434,-0.155794689166463,
0.13190329084344));
#15819=CARTESIAN_POINT('Ctrl Pts',(0.107368699171666,-0.12094033522185,
0.139842280480747));
#15820=CARTESIAN_POINT('Ctrl Pts',(0.15983782968835,0.0246266142906177,
0.147781270118052));
#15821=CARTESIAN_POINT('Ctrl Pts',(0.0659863808909888,0.147649582370873,
0.155720259755358));
#15822=CARTESIAN_POINT('Ctrl Pts',(-0.0882710769349216,0.135509478890084,
0.163659249392663));
#15823=CARTESIAN_POINT('Ctrl Pts',(-0.161722413615419,-0.00068026650363694,
0.171598239029969));
#15824=CARTESIAN_POINT('Ctrl Pts',(-0.0871279640988751,-0.136247273976568,
0.179537228667275));
#15825=CARTESIAN_POINT('Ctrl Pts',(0.0672261652318651,-0.147089240053593,
0.187476218304581));
#15826=CARTESIAN_POINT('Ctrl Pts',(0.160039347628626,-0.023281087390596,
0.195415207941886));
#15827=CARTESIAN_POINT('Ctrl Pts',(0.106347475470598,0.121839305139765,
0.203354197579192));
#15828=CARTESIAN_POINT('Ctrl Pts',(-0.0446982220051161,0.15542416405057,
0.211293187216498));
#15829=CARTESIAN_POINT('Ctrl Pts',(-0.154825760608133,0.0467288526640558,
0.219232176853804));
#15830=CARTESIAN_POINT('Ctrl Pts',(-0.12322092627477,-0.104743520787053,
0.227171166491109));
#15831=CARTESIAN_POINT('Ctrl Pts',(0.0211842211805034,-0.160330379506191,
0.235110156128415));
#15832=CARTESIAN_POINT('Ctrl Pts',(0.146196665995071,-0.0691457639426259,
0.24304914576572));
#15833=CARTESIAN_POINT('Ctrl Pts',(0.137376082602736,0.0853370596399817,
0.250988135403027));
#15834=CARTESIAN_POINT('Ctrl Pts',(0.00279711058556459,0.161699653653757,
0.258927125040332));
#15835=CARTESIAN_POINT('Ctrl Pts',(-0.134342424474264,0.0900372967480426,
0.266866114677638));
#15836=CARTESIAN_POINT('Ctrl Pts',(-0.148500677015507,-0.0640480346713102,
0.274805104314944));
#15837=CARTESIAN_POINT('Ctrl Pts',(-0.0267167371651392,-0.159501779847699,
0.282744093952249));
#15838=CARTESIAN_POINT('Ctrl Pts',(0.119524544542348,-0.108942576944327,
0.290683083589556));
#15839=CARTESIAN_POINT('Ctrl Pts',(0.156349297273321,0.0413460888291301,
0.29862207322686));
#15840=CARTESIAN_POINT('Ctrl Pts',(0.0500469836677093,0.153785243912065,
0.306561062864167));
#15841=CARTESIAN_POINT('Ctrl Pts',(-0.102069913541897,0.125444547784578,
0.314500052501472));
#15842=CARTESIAN_POINT('Ctrl Pts',(-0.160748800211922,-0.0177320345633525,
0.322439042138778));
#15843=CARTESIAN_POINT('Ctrl Pts',(-0.0722731771226978,-0.144676154524232,
0.330378031776084));
#15844=CARTESIAN_POINT('Ctrl Pts',(0.082363586418043,-0.139179170322594,
0.338317021413389));
#15845=CARTESIAN_POINT('Ctrl Pts',(0.16160213133829,-0.00627319426210969,
0.346256011050695));
#15846=CARTESIAN_POINT('Ctrl Pts',(0.0929050003357002,0.132375461215256,
0.354195000688001));
#15847=CARTESIAN_POINT('Ctrl Pts',(-0.0608402912787218,0.149843454232904,
0.362133990325306));
#15848=CARTESIAN_POINT('Ctrl Pts',(-0.158890465884947,0.0301400343429239,
0.370072979962613));
#15849=CARTESIAN_POINT('Ctrl Pts',(-0.1114873084483,-0.117154521356547,
0.378011969599918));
#15850=CARTESIAN_POINT('Ctrl Pts',(0.0379748391485164,-0.157202141877815,
0.385950959237223));
#15851=CARTESIAN_POINT('Ctrl Pts',(0.152673624090564,-0.0533419752763387,
0.39388994887453));
#15852=CARTESIAN_POINT('Ctrl Pts',(0.127610169584502,0.0993491139263089,
0.401828938511835));
#15853=CARTESIAN_POINT('Ctrl Pts',(-0.014271649480085,0.16109289816887,
0.409767928149142));
#15854=CARTESIAN_POINT('Ctrl Pts',(-0.143088751545671,0.0753671745551693,
0.417706917786446));
#15855=CARTESIAN_POINT('Ctrl Pts',(-0.140917908083783,-0.0793520321139836,
0.425645907423752));
#15856=CARTESIAN_POINT('Ctrl Pts',(-0.00974637750615997,-0.161429891732714,
0.433584897061058));
#15857=CARTESIAN_POINT('Ctrl Pts',(0.130347293715478,-0.0957297489831606,
0.441523886698364));
#15858=CARTESIAN_POINT('Ctrl Pts',(0.15111695082405,0.0576044181723055,
0.449462876335669));
#15859=CARTESIAN_POINT('Ctrl Pts',(0.0335493961742207,0.158205688379633,
0.457401865972975));
#15860=CARTESIAN_POINT('Ctrl Pts',(-0.114730331382826,0.113980493419335,
0.465340855610281));
#15861=CARTESIAN_POINT('Ctrl Pts',(-0.157982303542021,-0.03458603167299,
0.473279845247587));
#15862=CARTESIAN_POINT('Ctrl Pts',(-0.0566123040428622,-0.151491415104245,
0.481218834884892));
#15863=CARTESIAN_POINT('Ctrl Pts',(0.0965823799129518,-0.129716790392294,
0.489157824522198));
#15864=CARTESIAN_POINT('Ctrl Pts',(0.161362514281243,0.0108046658515635,
0.497096814159504));
#15865=CARTESIAN_POINT('Ctrl Pts',(0.0784263257203939,0.141435191000425,
0.50503580379681));
#15866=CARTESIAN_POINT('Ctrl Pts',(-0.076303789130349,0.14259149197508,
0.512974793434115));
#15867=CARTESIAN_POINT('Ctrl Pts',(-0.161183014472451,0.0132150544797126,
0.520913783071421));
#15868=CARTESIAN_POINT('Ctrl Pts',(-0.0985102366584373,-0.128258859705,
0.528852772708727));
#15869=CARTESIAN_POINT('Ctrl Pts',(0.0543419114689404,-0.152320577983508,
0.536791762346032));
#15870=CARTESIAN_POINT('Ctrl Pts',(0.157447763940923,-0.0369432463290883,
0.544730751983338));
#15871=CARTESIAN_POINT('Ctrl Pts',(0.116420979124965,0.112253095453589,
0.552669741620643));
#15872=CARTESIAN_POINT('Ctrl Pts',(-0.0311812332291155,0.158689421555565,
0.56060873125795));
#15873=CARTESIAN_POINT('Ctrl Pts',(-0.150239163551416,0.0598564579197502,
0.568547720895255));
#15874=CARTESIAN_POINT('Ctrl Pts',(-0.131763436204723,-0.0937709907106254,
0.576486710532561));
#15875=CARTESIAN_POINT('Ctrl Pts',(0.00733268664935855,-0.161557523891122,
0.584425700169866));
#15876=CARTESIAN_POINT('Ctrl Pts',(0.139716237417787,-0.0814492162095161,
0.592364689807173));
#15877=CARTESIAN_POINT('Ctrl Pts',(0.144199148209332,0.0732202668325601,
0.600303679444478));
#15878=CARTESIAN_POINT('Ctrl Pts',(0.0166776214282734,0.160861613702037,
0.608242669081784));
#15879=CARTESIAN_POINT('Ctrl Pts',(-0.126111124778327,0.101245177793678,
0.616181658719089));
#15880=CARTESIAN_POINT('Ctrl Pts',(-0.153453779210204,-0.0510542795996006,
0.624120648356396));
#15881=CARTESIAN_POINT('Ctrl Pts',(-0.0403200156494649,-0.156617042997737,
0.6320596379937));
#15882=CARTESIAN_POINT('Ctrl Pts',(0.10972395892722,-0.118807637198397,
0.639998627631007));
#15883=CARTESIAN_POINT('Ctrl Pts',(0.159323168980049,0.0277620180369333,
0.647937617268312));
#15884=CARTESIAN_POINT('Ctrl Pts',(0.0630729369615192,0.148917448414806,
0.655876606905618));
#15885=CARTESIAN_POINT('Ctrl Pts',(-0.0909162461746061,0.133749160748195,
0.663815596542924));
#15886=CARTESIAN_POINT('Ctrl Pts',(-0.161677836835157,-0.00385731715476066,
0.671754586180229));
#15887=CARTESIAN_POINT('Ctrl Pts',(-0.0844344483789265,-0.137932685561743,
0.679693575817536));
#15888=CARTESIAN_POINT('Ctrl Pts',(0.0701028908975481,-0.145740133481257,
0.687632565454841));
#15889=CARTESIAN_POINT('Ctrl Pts',(0.1604658380222,-0.0201324774223393,
0.695571555092147));
#15890=CARTESIAN_POINT('Ctrl Pts',(0.10393330787963,0.123905081947942,0.703510544729453));
#15891=CARTESIAN_POINT('Ctrl Pts',(-0.0477430426119635,0.15451603056473,
0.711449534366758));
#15892=CARTESIAN_POINT('Ctrl Pts',(-0.155713909636705,0.0436781428746717,
0.719388524004064));
#15893=CARTESIAN_POINT('Ctrl Pts',(-0.121139364160222,-0.10714409115852,
0.72732751364137));
#15894=CARTESIAN_POINT('Ctrl Pts',(0.0243299669821161,-0.159883252800214,
0.735266503278675));
#15895=CARTESIAN_POINT('Ctrl Pts',(0.147526880793862,-0.0662602540182413,
0.743205492915981));
#15896=CARTESIAN_POINT('Ctrl Pts',(0.135673045916277,0.0880194662056535,
0.751144482553287));
#15897=CARTESIAN_POINT('Ctrl Pts',(-0.000380164216571841,0.161723397486253,
0.759083472190592));
#15898=CARTESIAN_POINT('Ctrl Pts',(-0.136085360063504,0.0873806419964673,
0.767022461827899));
#15899=CARTESIAN_POINT('Ctrl Pts',(-0.147213735311121,-0.0669531026545853,
0.774961451465203));
#15900=CARTESIAN_POINT('Ctrl Pts',(-0.023578025097595,-0.159995870421162,
0.78290044110251));
#15901=CARTESIAN_POINT('Ctrl Pts',(0.121641751185188,-0.106573384050283,
0.790839430739816));
#15902=CARTESIAN_POINT('Ctrl Pts',(0.155506840911589,0.0444097314676148,
0.798778420377121));
#15903=CARTESIAN_POINT('Ctrl Pts',(0.047016075363265,0.15473878142458,0.806717410014428));
#15904=CARTESIAN_POINT('Ctrl Pts',(-0.104514684958047,0.123415081928621,
0.814656399651731));
#15905=CARTESIAN_POINT('Ctrl Pts',(-0.16036941405942,-0.020886666885039,
0.82259538928904));
#15906=CARTESIAN_POINT('Ctrl Pts',(-0.0694169354231278,-0.146068103622213,
0.830534378926343));
#15907=CARTESIAN_POINT('Ctrl Pts',(0.085081990139753,-0.137534202194171,
0.838473368563651));
#15908=CARTESIAN_POINT('Ctrl Pts',(0.161694184779289,-0.00309716449182502,
0.846412358200955));
#15909=CARTESIAN_POINT('Ctrl Pts',(0.0902864348795877,0.134175115040242,
0.854351347838261));
#15910=CARTESIAN_POINT('Ctrl Pts',(-0.0637723584188847,0.148619272374149,
0.862290337475567));
#15911=CARTESIAN_POINT('Ctrl Pts',(-0.159451928190027,0.0270126713934565,
0.870229327112872));
#15912=CARTESIAN_POINT('Ctrl Pts',(-0.109164185657521,-0.119322178948671,
0.878168316750179));
#15913=CARTESIAN_POINT('Ctrl Pts',(0.0410558873341998,-0.156425752146281,
0.886107306387484));
#15914=CARTESIAN_POINT('Ctrl Pts',(0.153692109215179,-0.0503322698109037,
0.894046296024789));
#15915=CARTESIAN_POINT('Ctrl Pts',(0.125633738317809,0.101836956040625,
0.901985285662096));
#15916=CARTESIAN_POINT('Ctrl Pts',(-0.0174337097671096,0.160781427979367,
0.909924275299401));
#15917=CARTESIAN_POINT('Ctrl Pts',(-0.144541791370401,0.072541521673891,
0.917863264936708));
#15918=CARTESIAN_POINT('Ctrl Pts',(-0.13933176907,-0.082105176128868,0.925802254574012));
#15919=CARTESIAN_POINT('Ctrl Pts',(-0.00657306121577474,-0.161590212220858,
0.933741244211319));
#15920=CARTESIAN_POINT('Ctrl Pts',(0.132202833700187,-0.0931504835251481,
0.941680233848624));
#15921=CARTESIAN_POINT('Ctrl Pts',(0.149956094815541,0.0605621288182698,
0.949619223485929));
#15922=CARTESIAN_POINT('Ctrl Pts',(0.0304348282896272,0.158834262822317,
0.957558213123236));
#15923=CARTESIAN_POINT('Ctrl Pts',(-0.116947437700435,0.111704514835484,
0.965497202760542));
#15924=CARTESIAN_POINT('Ctrl Pts',(-0.157272339407096,-0.0376830608728604,
0.973436192397847));
#15925=CARTESIAN_POINT('Ctrl Pts',(-0.0536251929639052,-0.152574376940928,
0.981375182035153));
#15926=CARTESIAN_POINT('Ctrl Pts',(0.0991121424632477,-0.127794307524525,
0.989314171672459));
#15927=CARTESIAN_POINT('Ctrl Pts',(0.161119104064031,0.0139726921146952,
0.997253161309763));
#15928=CARTESIAN_POINT('Ctrl Pts',(0.0756325681075411,0.142948649734045,
1.00519215094707));
#15929=CARTESIAN_POINT('Ctrl Pts',(-0.0790904005129918,0.141064915432658,
1.01313114058437));
#15930=CARTESIAN_POINT('Ctrl Pts',(-0.161411527883023,0.0100459188627121,
1.02107013022168));
#15931=CARTESIAN_POINT('Ctrl Pts',(-0.095971463730607,-0.130169427934261,
1.02900911985899));
#15932=CARTESIAN_POINT('Ctrl Pts',(0.0573238981132153,-0.151223584550935,
1.03694810949629));
#15933=CARTESIAN_POINT('Ctrl Pts',(0.158143159897702,-0.0338429135403315,
1.0448870991336));
#15934=CARTESIAN_POINT('Ctrl Pts',(0.114193197054413,0.114518625410106,
1.0528260887709));
#15935=CARTESIAN_POINT('Ctrl Pts',(-0.0342928115212847,0.158046211271557,
1.06076507840821));
#15936=CARTESIAN_POINT('Ctrl Pts',(-0.151386101389109,0.0568933223281485,
1.06870406804552));
#15937=CARTESIAN_POINT('Ctrl Pts',(-0.129895790602315,-0.0963415040526547,
1.07664305768282));
#15938=CARTESIAN_POINT('Ctrl Pts',(0.0105052141409744,-0.161382286187737,
1.08458204732013));
#15939=CARTESIAN_POINT('Ctrl Pts',(0.141289415307547,-0.0786886455683398,
1.09252103695743));
#15940=CARTESIAN_POINT('Ctrl Pts',(0.14273283995608,0.076039057183793,1.10046002659474));
#15941=CARTESIAN_POINT('Ctrl Pts',(0.013514131745196,0.161158214381091,
1.10839901623204));
#15942=CARTESIAN_POINT('Ctrl Pts',(-0.128075837894479,0.0987480712062529,
1.11633800586935));
#15943=CARTESIAN_POINT('Ctrl Pts',(-0.152421155552179,-0.0540591635106084,
1.12427699550666));
#15944=CARTESIAN_POINT('Ctrl Pts',(-0.0372353514058616,-0.157378938949945,
1.13221598514396));
#15945=CARTESIAN_POINT('Ctrl Pts',(0.11203686504723,-0.116629081663695,
1.14015497478127));
#15946=CARTESIAN_POINT('Ctrl Pts',(0.158747009937404,0.0308867067726846,
1.14809396441857));
#15947=CARTESIAN_POINT('Ctrl Pts',(0.0601351468730053,0.150127831962932,
1.15603295405588));
#15948=CARTESIAN_POINT('Ctrl Pts',(-0.0935263218228598,0.13193721592339,
1.16397194369318));
#15949=CARTESIAN_POINT('Ctrl Pts',(-0.161570852667341,-0.00703287904607843,
1.17191093333049));
#15950=CARTESIAN_POINT('Ctrl Pts',(-0.0817083410685703,-0.13956485524354,
1.17984992296779));
#15951=CARTESIAN_POINT('Ctrl Pts',(0.0729525569401478,-0.144334771469742,
1.1877889126051));
#15952=CARTESIAN_POINT('Ctrl Pts',(0.160830388835411,-0.016976096323307,
1.19572790224241));
#15953=CARTESIAN_POINT('Ctrl Pts',(0.101479022178261,0.125923031559255,
1.20366689187971));
#15954=CARTESIAN_POINT('Ctrl Pts',(-0.0507694344715009,0.153548254118279,
1.21160588151702));
#15955=CARTESIAN_POINT('Ctrl Pts',(-0.15654195331917,0.0406105733811438,
1.21954487115432));
#15956=CARTESIAN_POINT('Ctrl Pts',(-0.119011042423884,-0.109503304062093,
1.22748386079163));
#15957=CARTESIAN_POINT('Ctrl Pts',(0.0274663214511058,-0.159374411387982,
1.23542285042894));
#15958=CARTESIAN_POINT('Ctrl Pts',(0.148800150427453,-0.0633491677300162,
1.24336184006624));
#15959=CARTESIAN_POINT('Ctrl Pts',(0.133917639627974,0.0906678973829495,
1.25130082970354));
#15960=CARTESIAN_POINT('Ctrl Pts',(-0.00355729227603857,0.161684716318317,
1.25923981934086));
#15961=CARTESIAN_POINT('Ctrl Pts',(-0.137775766897813,0.0846902584421788,
1.26717880897816));
#15962=CARTESIAN_POINT('Ctrl Pts',(-0.14586996931591,-0.0698323268364953,
1.27511779861547));
#15963=CARTESIAN_POINT('Ctrl Pts',(-0.0204302119447119,-0.160428202816007,
1.28305678825277));
#15964=CARTESIAN_POINT('Ctrl Pts',(0.123712004283314,-0.104163053984564,
1.29099577789008));
#15965=CARTESIAN_POINT('Ctrl Pts',(0.15460435913624,0.0474562320176185,
1.29893476752738));
#15966=CARTESIAN_POINT('Ctrl Pts',(0.043967018911749,0.155632589980133,
1.30687375716469));
#15967=CARTESIAN_POINT('Ctrl Pts',(-0.106919113837756,0.121337978043289,
1.31481274680199));
#15968=CARTESIAN_POINT('Ctrl Pts',(-0.159928125575155,-0.0240332370134145,
1.3227517364393));
#15969=CARTESIAN_POINT('Ctrl Pts',(-0.0665338988230771,-0.147403670583407,
1.33069072607661));
#15970=CARTESIAN_POINT('Ctrl Pts',(0.0877675522160205,-0.135836146169277,
1.33862971571391));
#15971=CARTESIAN_POINT('Ctrl Pts',(0.161723824721502,8.00609866524728E-5,
1.34656870535122));
#15972=CARTESIAN_POINT('Ctrl Pts',(0.0876330185603928,0.135922977069285,
1.35450769498852));
#15973=CARTESIAN_POINT('Ctrl Pts',(-0.0666798087068602,0.147337724435113,
1.36244668462583));
#15974=CARTESIAN_POINT('Ctrl Pts',(-0.159951843822013,0.0238748801740983,
1.37038567426313));
#15975=CARTESIAN_POINT('Ctrl Pts',(-0.106798922716859,-0.121443775659372,
1.37832466390044));
#15976=CARTESIAN_POINT('Ctrl Pts',(0.0441210824430389,-0.155588987406456,
1.38626365353774));
#15977=CARTESIAN_POINT('Ctrl Pts',(0.154651279966657,-0.0473031264624986,
1.39420264317505));
#15978=CARTESIAN_POINT('Ctrl Pts',(0.123608792556459,0.10428547082216,1.40214163281236));
#15979=CARTESIAN_POINT('Ctrl Pts',(-0.020589002599541,0.160407931346284,
1.41008062244966));
#15980=CARTESIAN_POINT('Ctrl Pts',(-0.145939110542184,0.0696878015005003,
1.41801961208697));
#15981=CARTESIAN_POINT('Ctrl Pts',(-0.137691710982408,-0.0848265016612731,
1.42595860172427));
#15982=CARTESIAN_POINT('Ctrl Pts',(-0.00339746822928561,-0.161688398335044,
1.43389759136158));
#15983=CARTESIAN_POINT('Ctrl Pts',(0.134007838137522,-0.0905348079547059,
1.44183658099889));
#15984=CARTESIAN_POINT('Ctrl Pts',(0.148736417039967,0.0634956003383226,
1.44977557063619));
#15985=CARTESIAN_POINT('Ctrl Pts',(0.0273102951854726,0.159403164432859,
1.4577145602735));
#15986=CARTESIAN_POINT('Ctrl Pts',(-0.119122786779006,0.109382310628272,
1.4656535499108));
#15987=CARTESIAN_POINT('Ctrl Pts',(-0.156495242883694,-0.0407596439572756,
1.47359253954811));
#15988=CARTESIAN_POINT('Ctrl Pts',(-0.0506295842364637,-0.153609649276743,
1.48153152918541));
#15989=CARTESIAN_POINT('Ctrl Pts',(0.10162683549218,-0.125801210382132,
1.48947051882272));
#15990=CARTESIAN_POINT('Ctrl Pts',(0.160769288057966,0.017094787472962,
1.49740950846002));
#15991=CARTESIAN_POINT('Ctrl Pts',(0.0728951834924312,0.144484958595688,
1.50534849809733));
#15992=CARTESIAN_POINT('Ctrl Pts',(-0.0820226078184241,0.139326700971572,
1.51328748773464));
#15993=CARTESIAN_POINT('Ctrl Pts',(-0.134767702434085,0.0512744806661359,
1.51858014749284));
#15994=CARTESIAN_POINT('Ctrl Pts',(-0.136701386950156,0.00581475974600206,
1.52122647737194));
#15995=CARTESIAN_POINT('Ctrl Pts',(0.0740036351041134,-0.103579689087085,
-0.0054992613140312));
#15996=CARTESIAN_POINT('Ctrl Pts',(0.108448814220036,-0.0789699563406641,
-0.00285293143492929));
#15997=CARTESIAN_POINT('Ctrl Pts',(0.150264871169078,0.00688399744800666,
0.00243972832327453));
#15998=CARTESIAN_POINT('Ctrl Pts',(0.0755551489391376,0.130236700260234,
0.0103787179605803));
#15999=CARTESIAN_POINT('Ctrl Pts',(-0.0683810376584167,0.133979098529349,
0.0183177075978859));
#16000=CARTESIAN_POINT('Ctrl Pts',(-0.14968704878538,0.0152677557027674,
0.0262566972351917));
#16001=CARTESIAN_POINT('Ctrl Pts',(-0.0939816891590436,-0.11752176362514,
0.0341956868724974));
#16002=CARTESIAN_POINT('Ctrl Pts',(0.0477663481097245,-0.142674779628989,
0.0421346765098031));
#16003=CARTESIAN_POINT('Ctrl Pts',(0.14578288888032,-0.0372469160898187,
0.0500736661471088));
#16004=CARTESIAN_POINT('Ctrl Pts',(0.110347650287512,0.102292747252513,
0.0580126557844146));
#16005=CARTESIAN_POINT('Ctrl Pts',(-0.0261045975097209,0.148182615303324,
0.0659516454217203));
#16006=CARTESIAN_POINT('Ctrl Pts',(-0.13865919166998,0.0584255608647477,
0.073890635059026));
#16007=CARTESIAN_POINT('Ctrl Pts',(-0.124281158904105,-0.0848182532198701,
0.0818296246963318));
#16008=CARTESIAN_POINT('Ctrl Pts',(0.00386794697500161,-0.15041563023346,
0.0897686143336374));
#16009=CARTESIAN_POINT('Ctrl Pts',(0.128476112576568,-0.0783184064825255,
0.0977076039709433));
#16010=CARTESIAN_POINT('Ctrl Pts',(0.135473254782295,0.0654742669580799,
0.105646593608249));
#16011=CARTESIAN_POINT('Ctrl Pts',(0.0184538891044151,0.149329569763132,
0.113585583245555));
#16012=CARTESIAN_POINT('Ctrl Pts',(-0.115458732720671,0.096483973363118,
0.12152457288286));
#16013=CARTESIAN_POINT('Ctrl Pts',(-0.143676805334049,-0.0446861343604874,
0.129463562520166));
#16014=CARTESIAN_POINT('Ctrl Pts',(-0.0403686054279526,-0.144949124289353,
0.137402552157472));
#16015=CARTESIAN_POINT('Ctrl Pts',(0.0998942839726139,-0.112521137758025,
0.145341541794778));
#16016=CARTESIAN_POINT('Ctrl Pts',(0.14871080372247,0.0229122455632766,
0.153280531432083));
#16017=CARTESIAN_POINT('Ctrl Pts',(0.0613927738894439,0.137371034794898,
0.161219521069389));
#16018=CARTESIAN_POINT('Ctrl Pts',(-0.0821261326059948,0.126076058196294,
0.169158510706695));
#16019=CARTESIAN_POINT('Ctrl Pts',(-0.150464193336327,-0.000632910110818063,
0.177097500344));
#16020=CARTESIAN_POINT('Ctrl Pts',(-0.0810625969653723,-0.126762492068094,
0.185036489981306));
#16021=CARTESIAN_POINT('Ctrl Pts',(0.0625462512992226,-0.136849700411639,
0.192975479618612));
#16022=CARTESIAN_POINT('Ctrl Pts',(0.148898293097928,-0.0216603868066741,
0.200914469255917));
#16023=CARTESIAN_POINT('Ctrl Pts',(0.0989441522193119,0.113357526360621,
0.208853458893223));
#16024=CARTESIAN_POINT('Ctrl Pts',(-0.0415865789238149,0.144604393083411,
0.216792448530529));
#16025=CARTESIAN_POINT('Ctrl Pts',(-0.144047647180085,0.0434758483035601,
0.224731438167835));
#16026=CARTESIAN_POINT('Ctrl Pts',(-0.114642966671137,-0.0974518559926297,
0.232670427805141));
#16027=CARTESIAN_POINT('Ctrl Pts',(0.0197094928286333,-0.149169064945282,
0.240609417442446));
#16028=CARTESIAN_POINT('Ctrl Pts',(0.136019262424063,-0.0643322181611298,
0.248548407079752));
#16029=CARTESIAN_POINT('Ctrl Pts',(0.127812719278849,0.0793963653730636,
0.256487396717058));
#16030=CARTESIAN_POINT('Ctrl Pts',(0.00260239121171357,0.150443017797356,
0.264426386354363));
#16031=CARTESIAN_POINT('Ctrl Pts',(-0.124990247656303,0.0837693979610897,
0.272365375991669));
#16032=CARTESIAN_POINT('Ctrl Pts',(-0.138162880936044,-0.0595893646165358,
0.280304365628975));
#16033=CARTESIAN_POINT('Ctrl Pts',(-0.0248568656394851,-0.148398147813718,
0.288243355266281));
#16034=CARTESIAN_POINT('Ctrl Pts',(0.111203906597776,-0.101358597076653,
0.296182344903586));
#16035=CARTESIAN_POINT('Ctrl Pts',(0.145465123646218,0.0384678027257296,
0.304121334540892));
#16036=CARTESIAN_POINT('Ctrl Pts',(0.0465629893725541,0.143079565503422,
0.312060324178198));
#16037=CARTESIAN_POINT('Ctrl Pts',(-0.0949643705016135,0.116711791945748,
0.319999313815503));
#16038=CARTESIAN_POINT('Ctrl Pts',(-0.149558357514911,-0.0164976283567656,
0.327938303452809));
#16039=CARTESIAN_POINT('Ctrl Pts',(-0.0672419181269484,-0.134604600554976,
0.335877293090115));
#16040=CARTESIAN_POINT('Ctrl Pts',(0.0766298889166206,-0.12949028600085,
0.343816282727421));
#16041=CARTESIAN_POINT('Ctrl Pts',(0.150352284446295,-0.00583648916182633,
0.351755272364726));
#16042=CARTESIAN_POINT('Ctrl Pts',(0.0864374678803939,0.123160213504125,
0.359694262002032));
#16043=CARTESIAN_POINT('Ctrl Pts',(-0.0566049265834532,0.139412181427728,
0.367633251639338));
#16044=CARTESIAN_POINT('Ctrl Pts',(-0.147829390149123,0.0280418517950267,
0.375572241276644));
#16045=CARTESIAN_POINT('Ctrl Pts',(-0.103726178443039,-0.108998871322406,
0.383511230913949));
#16046=CARTESIAN_POINT('Ctrl Pts',(0.0353312408083745,-0.146258597924691,
0.391450220551255));
#16047=CARTESIAN_POINT('Ctrl Pts',(0.142045330507792,-0.0496286018832686,
0.399389210188561));
#16048=CARTESIAN_POINT('Ctrl Pts',(0.118726655129599,0.0924329779120693,
0.407328199825866));
#16049=CARTESIAN_POINT('Ctrl Pts',(-0.0132781361506635,0.1498785012746,
0.415267189463172));
#16050=CARTESIAN_POINT('Ctrl Pts',(-0.133127703795094,0.0701205285647604,
0.423206179100478));
#16051=CARTESIAN_POINT('Ctrl Pts',(-0.131107982452518,-0.0738279823724454,
0.431145168737783));
#16052=CARTESIAN_POINT('Ctrl Pts',(-0.00906788859151817,-0.150192035209753,
0.439084158375089));
#16053=CARTESIAN_POINT('Ctrl Pts',(0.121273235812024,-0.0890655731449414,
0.447023148012395));
#16054=CARTESIAN_POINT('Ctrl Pts',(0.14059702422731,0.0535943170716914,
0.4549621376497));
#16055=CARTESIAN_POINT('Ctrl Pts',(0.031213872705855,0.14719228306762,0.462901127287006));
#16056=CARTESIAN_POINT('Ctrl Pts',(-0.106743440051405,0.106045801661112,
0.470840116924312));
#16057=CARTESIAN_POINT('Ctrl Pts',(-0.146984449047318,-0.0321783433727119,
0.478779106561618));
#16058=CARTESIAN_POINT('Ctrl Pts',(-0.0526712684425847,-0.140945420374714,
0.486718096198923));
#16059=CARTESIAN_POINT('Ctrl Pts',(0.0898588486235595,-0.120686624644175,
0.49465708583623));
#16060=CARTESIAN_POINT('Ctrl Pts',(0.150129348203927,0.0100525047535443,
0.502596075473534));
#16061=CARTESIAN_POINT('Ctrl Pts',(0.0729667185397875,0.131589254992538,
0.510535065110842));
#16062=CARTESIAN_POINT('Ctrl Pts',(-0.0709919412117167,0.132665060686482,
0.518474054748145));
#16063=CARTESIAN_POINT('Ctrl Pts',(-0.149962344179375,0.0122950954523496,
0.526413044385453));
#16064=CARTESIAN_POINT('Ctrl Pts',(-0.0916524986414713,-0.119330187030486,
0.534352034022757));
#16065=CARTESIAN_POINT('Ctrl Pts',(0.0505589280467443,-0.141716861518734,
0.542291023660064));
#16066=CARTESIAN_POINT('Ctrl Pts',(0.146487121137799,-0.0343714617774037,
0.550230013297369));
#16067=CARTESIAN_POINT('Ctrl Pts',(0.108316394245265,0.104438655591022,
0.558169002934674));
#16068=CARTESIAN_POINT('Ctrl Pts',(-0.0290105681715044,0.147642341414387,
0.566107992571982));
#16069=CARTESIAN_POINT('Ctrl Pts',(-0.139780343651344,0.0556895822633619,
0.574046982209285));
#16070=CARTESIAN_POINT('Ctrl Pts',(-0.122590794290966,-0.0872431727934394,
0.581985971846593));
#16071=CARTESIAN_POINT('Ctrl Pts',(0.00682222554696161,-0.150310782322966,
0.589924961483898));
#16072=CARTESIAN_POINT('Ctrl Pts',(0.129989965454297,-0.0757791721064987,
0.597863951121203));
#16073=CARTESIAN_POINT('Ctrl Pts',(0.134160800782372,0.0681230766876274,
0.60580294075851));
#16074=CARTESIAN_POINT('Ctrl Pts',(0.015516617634347,0.149663317553585,
0.613741930395814));
#16075=CARTESIAN_POINT('Ctrl Pts',(-0.117331965534667,0.0941970482962578,
0.621680920033121));
#16076=CARTESIAN_POINT('Ctrl Pts',(-0.142771175541451,-0.0475001629309618,
0.629619909670426));
#16077=CARTESIAN_POINT('Ctrl Pts',(-0.0375131590877193,-0.145714230393655,
0.637558899307733));
#16078=CARTESIAN_POINT('Ctrl Pts',(0.102085583566124,-0.110536906379362,
0.645497888945037));
#16079=CARTESIAN_POINT('Ctrl Pts',(0.148231970847143,0.0258293798362968,
0.653436878582344));
#16080=CARTESIAN_POINT('Ctrl Pts',(0.0586821478180281,0.138550639014834,
0.661375868219649));
#16081=CARTESIAN_POINT('Ctrl Pts',(-0.0845871597882484,0.124438283670714,
0.669314857856955));
#16082=CARTESIAN_POINT('Ctrl Pts',(-0.150422719745043,-0.00358879206139753,
0.67725384749426));
#16083=CARTESIAN_POINT('Ctrl Pts',(-0.078556588917505,-0.128330574617282,
0.685192837131567));
#16084=CARTESIAN_POINT('Ctrl Pts',(0.065222715229363,-0.135594511179713,
0.693131826768872));
#16085=CARTESIAN_POINT('Ctrl Pts',(0.149295093588351,-0.0187309656558678,
0.701070816406178));
#16086=CARTESIAN_POINT('Ctrl Pts',(0.0966980456281902,0.11527949520901,
0.709009806043483));
#16087=CARTESIAN_POINT('Ctrl Pts',(-0.044419435954706,0.14375947882982,
0.716948795680789));
#16088=CARTESIAN_POINT('Ctrl Pts',(-0.144873968183829,0.0406375120624596,
0.724887785318095));
#16089=CARTESIAN_POINT('Ctrl Pts',(-0.112706311402131,-0.099685311927494,
0.732826774955401));
#16090=CARTESIAN_POINT('Ctrl Pts',(0.0226362492002416,-0.148753064728429,
0.740765764592706));
#16091=CARTESIAN_POINT('Ctrl Pts',(0.137256875023267,-0.0616475814838108,
0.748704754230013));
#16092=CARTESIAN_POINT('Ctrl Pts',(0.126228238590478,0.0818920376245527,
0.756643743867318));
#16093=CARTESIAN_POINT('Ctrl Pts',(-0.000353699285724532,0.150465108715513,
0.764582733504624));
#16094=CARTESIAN_POINT('Ctrl Pts',(-0.126611849706441,0.0812976848247803,
0.772521723141928));
#16095=CARTESIAN_POINT('Ctrl Pts',(-0.136965528997667,-0.0622921978288208,
0.780460712779236));
#16096=CARTESIAN_POINT('Ctrl Pts',(-0.0219366533522686,-0.148857842533265,
0.788399702416541));
#16097=CARTESIAN_POINT('Ctrl Pts',(0.113173725020093,-0.0991543342927188,
0.796338692053846));
#16098=CARTESIAN_POINT('Ctrl Pts',(0.144681314438483,0.0413181715024817,
0.804277681691154));
#16099=CARTESIAN_POINT('Ctrl Pts',(0.0437430761464933,0.143966723006387,
0.812216671328456));
#16100=CARTESIAN_POINT('Ctrl Pts',(-0.0972389504488157,0.114823606281847,
0.820155660965765));
#16101=CARTESIAN_POINT('Ctrl Pts',(-0.149205382128735,-0.0194326526180533,
0.828094650603069));
#16102=CARTESIAN_POINT('Ctrl Pts',(-0.0645845121824554,-0.135899649852787,
0.836033640240376));
#16103=CARTESIAN_POINT('Ctrl Pts',(0.0791590524011713,-0.127959831458565,
0.843972629877681));
#16104=CARTESIAN_POINT('Ctrl Pts',(0.150437929635691,-0.00288155702400619,
0.851911619514986));
#16105=CARTESIAN_POINT('Ctrl Pts',(0.0840011924733913,0.12483458538003,
0.859850609152293));
#16106=CARTESIAN_POINT('Ctrl Pts',(-0.0593328794206009,0.138273220341526,
0.867789598789597));
#16107=CARTESIAN_POINT('Ctrl Pts',(-0.148351766552825,0.0251321985630355,
0.875728588426904));
#16108=CARTESIAN_POINT('Ctrl Pts',(-0.1015647786165,-0.111015628577859,
0.883667578064211));
#16109=CARTESIAN_POINT('Ctrl Pts',(0.0381978034543637,-0.145536256153639,
0.891606567701514));
#16110=CARTESIAN_POINT('Ctrl Pts',(0.142992914329196,-0.046828415471795,
0.899545557338823));
#16111=CARTESIAN_POINT('Ctrl Pts',(0.116887812080083,0.0947476302135675,
0.907484546976125));
#16112=CARTESIAN_POINT('Ctrl Pts',(-0.0162200712834111,0.149588713917584,
0.915423536613434));
#16113=CARTESIAN_POINT('Ctrl Pts',(-0.134479591021026,0.067491582014154,
0.923362526250738));
#16114=CARTESIAN_POINT('Ctrl Pts',(-0.129632261667175,-0.0763894677230377,
0.931301515888044));
#16115=CARTESIAN_POINT('Ctrl Pts',(-0.00611548103612966,-0.150341195071919,
0.93924050552535));
#16116=CARTESIAN_POINT('Ctrl Pts',(0.122999603362204,-0.0866658618874593,
0.947179495162656));
#16117=CARTESIAN_POINT('Ctrl Pts',(0.139516980595786,0.0563461282555487,
0.95511848479996));
#16118=CARTESIAN_POINT('Ctrl Pts',(0.0283161238170646,0.147777099632969,
0.963057474437267));
#16119=CARTESIAN_POINT('Ctrl Pts',(-0.108806203685475,0.103928264122473,
0.970996464074573));
#16120=CARTESIAN_POINT('Ctrl Pts',(-0.146323908690103,-0.0350597745230392,
0.978935453711877));
#16121=CARTESIAN_POINT('Ctrl Pts',(-0.049892103521326,-0.14195299239598,
0.986874443349185));
#16122=CARTESIAN_POINT('Ctrl Pts',(0.0922125030920605,-0.118897974404329,
0.994813432986488));
#16123=CARTESIAN_POINT('Ctrl Pts',(0.149902882860231,0.0129999905441286,
1.0027524226238));
#16124=CARTESIAN_POINT('Ctrl Pts',(0.0703674468853664,0.132997355096976,
1.0106914122611));
#16125=CARTESIAN_POINT('Ctrl Pts',(-0.0735845641169637,0.131244755962562,
1.01863040189841));
#16126=CARTESIAN_POINT('Ctrl Pts',(-0.150174949749745,0.00934657753497952,
1.02656939153571));
#16127=CARTESIAN_POINT('Ctrl Pts',(-0.0892904610481016,-0.121107752063083,
1.03450838117302));
#16128=CARTESIAN_POINT('Ctrl Pts',(0.0533333252681307,-0.140696234703703,
1.04244737081032));
#16129=CARTESIAN_POINT('Ctrl Pts',(0.147134107472884,-0.031486957015783,
1.05038636044763));
#16130=CARTESIAN_POINT('Ctrl Pts',(0.106243698045146,0.106546471877992,
1.05832535008494));
#16131=CARTESIAN_POINT('Ctrl Pts',(-0.0319055355867657,0.147043907874068,
1.06626433972224));
#16132=CARTESIAN_POINT('Ctrl Pts',(-0.14084743801815,0.0529327237885883,
1.07420332935955));
#16133=CARTESIAN_POINT('Ctrl Pts',(-0.120853163849259,-0.0896347412088629,
1.08214231899685));
#16134=CARTESIAN_POINT('Ctrl Pts',(0.00977389921538986,-0.150147743699608,
1.09008130863416));
#16135=CARTESIAN_POINT('Ctrl Pts',(0.13145362739741,-0.0732107771302755,
1.09802029827146));
#16136=CARTESIAN_POINT('Ctrl Pts',(0.132796568802552,0.0707456384395876,
1.10595928790877));
#16137=CARTESIAN_POINT('Ctrl Pts',(0.0125733526121963,0.149939270533256,
1.11389827754607));
#16138=CARTESIAN_POINT('Ctrl Pts',(-0.119159906186493,0.0918737764630459,
1.12183726718338));
#16139=CARTESIAN_POINT('Ctrl Pts',(-0.141810437433163,-0.0502958634379693,
1.12977625682069));
#16140=CARTESIAN_POINT('Ctrl Pts',(-0.0346432321137694,-0.146423087362162,
1.13771524645799));
#16141=CARTESIAN_POINT('Ctrl Pts',(0.104237477950025,-0.108510009835838,
1.1456542360953));
#16142=CARTESIAN_POINT('Ctrl Pts',(0.147695920811486,0.0287365450185451,
1.1535932257326));
#16143=CARTESIAN_POINT('Ctrl Pts',(0.0559488704325515,0.139676762352502,
1.16153221536991));
#16144=CARTESIAN_POINT('Ctrl Pts',(-0.0870155364008756,0.12275247642644,
1.16947120500722));
#16145=CARTESIAN_POINT('Ctrl Pts',(-0.150323183223479,-0.00654328889139735,
1.17741019464452));
#16146=CARTESIAN_POINT('Ctrl Pts',(-0.0760202581255566,-0.129849121670035,
1.18534918428183));
#16147=CARTESIAN_POINT('Ctrl Pts',(0.0678740032777675,-0.134286982701248,
1.19328817391913));
#16148=CARTESIAN_POINT('Ctrl Pts',(0.149634266389533,-0.0157943143574443,
1.20122716355644));
#16149=CARTESIAN_POINT('Ctrl Pts',(0.0944146137277022,0.117156966325547,
1.20916615319374));
#16150=CARTESIAN_POINT('Ctrl Pts',(-0.047235147145783,0.142859073628774,
1.21710514283105));
#16151=CARTESIAN_POINT('Ctrl Pts',(-0.145644368043342,0.037783489796601,
1.22504413246835));
#16152=CARTESIAN_POINT('Ctrl Pts',(-0.11072615165767,-0.101880289472715,
1.23298312210566));
#16153=CARTESIAN_POINT('Ctrl Pts',(0.0255542680118797,-0.148279646041953,
1.24092211174296));
#16154=CARTESIAN_POINT('Ctrl Pts',(0.138441506664824,-0.0589391489276913,
1.24886110138027));
#16155=CARTESIAN_POINT('Ctrl Pts',(0.124595033982396,0.0843560996663564,
1.25680009101758));
#16156=CARTESIAN_POINT('Ctrl Pts',(-0.00330965325590636,0.150429120316621,
1.26473908065488));
#16157=CARTESIAN_POINT('Ctrl Pts',(-0.128184579763139,0.0787945908985174,
1.27267807029219));
#16158=CARTESIAN_POINT('Ctrl Pts',(-0.135715308561414,-0.0649709863423027,
1.2806170599295));
#16159=CARTESIAN_POINT('Ctrl Pts',(-0.0190079735469551,-0.149260078337129,
1.2885560495668));
#16160=CARTESIAN_POINT('Ctrl Pts',(0.115099858543875,-0.0969117980795561,
1.29649503920411));
#16161=CARTESIAN_POINT('Ctrl Pts',(0.143841658454547,0.0441525915281748,
1.30443402884141));
#16162=CARTESIAN_POINT('Ctrl Pts',(0.0409062781470196,0.144798309552134,
1.31237301847872));
#16163=CARTESIAN_POINT('Ctrl Pts',(-0.0994759962839106,0.112891098884786,
1.32031200811602));
#16164=CARTESIAN_POINT('Ctrl Pts',(-0.148794813708878,-0.0223601759313527,
1.32825099775333));
#16165=CARTESIAN_POINT('Ctrl Pts',(-0.0619021766503053,-0.13714224202644,
1.33618998739064));
#16166=CARTESIAN_POINT('Ctrl Pts',(0.0816576604940555,-0.126379984705639,
1.34412897702794));
#16167=CARTESIAN_POINT('Ctrl Pts',(0.150465506209006,7.4487583413377E-5,
1.35206796666525));
#16168=CARTESIAN_POINT('Ctrl Pts',(0.0815324923277053,0.126460770918471,
1.36000695630255));
#16169=CARTESIAN_POINT('Ctrl Pts',(-0.062037929094705,0.137080886684378,
1.36794594593986));
#16170=CARTESIAN_POINT('Ctrl Pts',(-0.148816880822527,0.0222128430196456,
1.37588493557716));
#16171=CARTESIAN_POINT('Ctrl Pts',(-0.0993641722043223,-0.112989531455785,
1.38382392521447));
#16172=CARTESIAN_POINT('Ctrl Pts',(0.0410496166270677,-0.144757742348562,
1.39176291485178));
#16173=CARTESIAN_POINT('Ctrl Pts',(0.143885312916173,-0.0440101443352923,
1.39970190448908));
#16174=CARTESIAN_POINT('Ctrl Pts',(0.115003831846793,0.0970256929337524,
1.40764089412639));
#16175=CARTESIAN_POINT('Ctrl Pts',(-0.0191557100743377,0.149241218055048,
1.41557988376369));
#16176=CARTESIAN_POINT('Ctrl Pts',(-0.135779636557791,0.0648365220611291,
1.423518873401));
#16177=CARTESIAN_POINT('Ctrl Pts',(-0.128106375355825,-0.0789213496179777,
1.4314578630383));
#16178=CARTESIAN_POINT('Ctrl Pts',(-0.00316095527563228,-0.150432546011701,
1.43939685267561));
#16179=CARTESIAN_POINT('Ctrl Pts',(0.12467895337041,-0.0842322751882648,
1.44733584231291));
#16180=CARTESIAN_POINT('Ctrl Pts',(0.138382210043398,0.0590753877074232,
1.45527483195022));
#16181=CARTESIAN_POINT('Ctrl Pts',(0.0254091034322018,0.148306397458819,
1.46321382158753));
#16182=CARTESIAN_POINT('Ctrl Pts',(-0.110830116988615,0.101767718932792,
1.47115281122483));
#16183=CARTESIAN_POINT('Ctrl Pts',(-0.145600909330124,-0.0379221829034233,
1.47909180086214));
#16184=CARTESIAN_POINT('Ctrl Pts',(-0.0471050325108872,-0.142916194795756,
1.48703079049945));
#16185=CARTESIAN_POINT('Ctrl Pts',(0.0945521370959566,-0.117043625665234,
1.49496978013675));
#16186=CARTESIAN_POINT('Ctrl Pts',(0.14957741911039,0.0159047428854941,
1.50290876977406));
#16187=CARTESIAN_POINT('Ctrl Pts',(0.0678206238522695,0.134426714629862,
1.51084775941136));
#16188=CARTESIAN_POINT('Ctrl Pts',(-0.0763126473618499,0.129627546381738,
1.51878674904867));
#16189=CARTESIAN_POINT('Ctrl Pts',(-0.125385920115907,0.0477050348167321,
1.52407940880687));
#16190=CARTESIAN_POINT('Ctrl Pts',(-0.127184992207234,0.00540996832206346,
1.52672573868597));
#16191=CARTESIAN_POINT('Ctrl Pts',(0.0684664424539414,-0.095829519891843,
-1.38777878078145E-17));
#16192=CARTESIAN_POINT('Ctrl Pts',(0.100334321247169,-0.0730611673843044,
0.00264632987910189));
#16193=CARTESIAN_POINT('Ctrl Pts',(0.139021564822767,0.00636891437108143,
0.00793898963730573));
#16194=CARTESIAN_POINT('Ctrl Pts',(0.0699018669780613,0.120491966796142,
0.0158779792746114));
#16195=CARTESIAN_POINT('Ctrl Pts',(-0.0632645460347191,0.123954346655885,
0.0238169689119172));
#16196=CARTESIAN_POINT('Ctrl Pts',(-0.138486976988987,0.0141253725679007,
0.0317559585492228));
#16197=CARTESIAN_POINT('Ctrl Pts',(-0.0869496735326521,-0.108728403071097,
0.0396949481865287));
#16198=CARTESIAN_POINT('Ctrl Pts',(0.0441923146003338,-0.131999388615902,
0.0476339378238343));
#16199=CARTESIAN_POINT('Ctrl Pts',(0.134874939024977,-0.034459980695041,
0.0555729274611401));
#16200=CARTESIAN_POINT('Ctrl Pts',(0.102091080224759,0.094638871230671,
0.0635119170984456));
#16201=CARTESIAN_POINT('Ctrl Pts',(-0.0241513666277066,0.137095110112719,
0.0714509067357516));
#16202=CARTESIAN_POINT('Ctrl Pts',(-0.128284260007319,0.0540539703915629,
0.0793898963730571));
#16203=CARTESIAN_POINT('Ctrl Pts',(-0.114982038412656,-0.0784718756714057,
0.0873288860103631));
#16204=CARTESIAN_POINT('Ctrl Pts',(0.00357853460314598,-0.139161043603659,
0.0952678756476685));
#16205=CARTESIAN_POINT('Ctrl Pts',(0.118863112008681,-0.0724583686054966,
0.103206865284975));
#16206=CARTESIAN_POINT('Ctrl Pts',(0.125336705278751,0.0605752693714656,
0.11114585492228));
#16207=CARTESIAN_POINT('Ctrl Pts',(0.0170731091066207,0.138156245709763,
0.119084844559586));
#16208=CARTESIAN_POINT('Ctrl Pts',(-0.106819734848208,0.0892647286947484,
0.127023834196891));
#16209=CARTESIAN_POINT('Ctrl Pts',(-0.132926439498961,-0.0413425724611633,
0.134962823834197));
#16210=CARTESIAN_POINT('Ctrl Pts',(-0.0373480950846616,-0.134103559412242,
0.142901813471503));
#16211=CARTESIAN_POINT('Ctrl Pts',(0.0924198687735613,-0.104101940294199,
0.150840803108809));
#16212=CARTESIAN_POINT('Ctrl Pts',(0.137583777756591,0.0211978768359354,
0.158779792746114));
#16213=CARTESIAN_POINT('Ctrl Pts',(0.0567991668878991,0.127092487218924,
0.16671878238342));
#16214=CARTESIAN_POINT('Ctrl Pts',(-0.075981188277068,0.116642637502503,
0.174657772020726));
#16215=CARTESIAN_POINT('Ctrl Pts',(-0.139205973057234,-0.000585553717998882,
0.182596761658032));
#16216=CARTESIAN_POINT('Ctrl Pts',(-0.0749972298318695,-0.11727771015962,
0.190535751295337));
#16217=CARTESIAN_POINT('Ctrl Pts',(0.0578663373665801,-0.126610160769685,
0.198474740932643));
#16218=CARTESIAN_POINT('Ctrl Pts',(0.13775723856723,-0.0200396862227523,
0.206413730569949));
#16219=CARTESIAN_POINT('Ctrl Pts',(0.091540828968026,0.104875747581476,
0.214352720207254));
#16220=CARTESIAN_POINT('Ctrl Pts',(-0.0384749358425138,0.133784622116252,
0.22229170984456));
#16221=CARTESIAN_POINT('Ctrl Pts',(-0.133269533752038,0.0402228439430644,
0.230230699481866));
#16222=CARTESIAN_POINT('Ctrl Pts',(-0.106065007067505,-0.0901601911982067,
0.238169689119172));
#16223=CARTESIAN_POINT('Ctrl Pts',(0.0182347644767634,-0.138007750384372,
0.246108678756477));
#16224=CARTESIAN_POINT('Ctrl Pts',(0.125841858853055,-0.0595186723796334,
0.254047668393783));
#16225=CARTESIAN_POINT('Ctrl Pts',(0.118249355954961,0.073455671106145,
0.261986658031089));
#16226=CARTESIAN_POINT('Ctrl Pts',(0.00240767183786234,0.139186381940956,
0.269925647668394));
#16227=CARTESIAN_POINT('Ctrl Pts',(-0.115638070838342,0.0775014991741366,
0.277864637305701));
#16228=CARTESIAN_POINT('Ctrl Pts',(-0.12782508485658,-0.0551306945617612,
0.285803626943006));
#16229=CARTESIAN_POINT('Ctrl Pts',(-0.0229969941138309,-0.137294515779738,
0.293742616580312));
#16230=CARTESIAN_POINT('Ctrl Pts',(0.102883268653204,-0.0937746172089793,
0.301681606217617));
#16231=CARTESIAN_POINT('Ctrl Pts',(0.134580950019115,0.0355895166223291,
0.309620595854923));
#16232=CARTESIAN_POINT('Ctrl Pts',(0.0430789950773988,0.13237388709478,
0.317559585492229));
#16233=CARTESIAN_POINT('Ctrl Pts',(-0.0878588274613298,0.107979036106918,
0.325498575129534));
#16234=CARTESIAN_POINT('Ctrl Pts',(-0.1383679148179,-0.0152632221501787,
0.33343756476684));
#16235=CARTESIAN_POINT('Ctrl Pts',(-0.0622106591311991,-0.12453304658572,
0.341376554404146));
#16236=CARTESIAN_POINT('Ctrl Pts',(0.0708961914151981,-0.119801401679107,
0.349315544041452));
#16237=CARTESIAN_POINT('Ctrl Pts',(0.1391024375543,-0.00539978406154301,
0.357254533678757));
#16238=CARTESIAN_POINT('Ctrl Pts',(0.0799699354250877,0.113944965792994,
0.365193523316063));
#16239=CARTESIAN_POINT('Ctrl Pts',(-0.0523695618881846,0.128980908622551,
0.373132512953369));
#16240=CARTESIAN_POINT('Ctrl Pts',(-0.136768314413298,0.0259436692471295,
0.381071502590675));
#16241=CARTESIAN_POINT('Ctrl Pts',(-0.0959650484377783,-0.100843221288265,
0.38901049222798));
#16242=CARTESIAN_POINT('Ctrl Pts',(0.0326876424682324,-0.135315053971568,
0.396949481865287));
#16243=CARTESIAN_POINT('Ctrl Pts',(0.13141703692502,-0.0459152284901983,
0.404888471502591));
#16244=CARTESIAN_POINT('Ctrl Pts',(0.109843140674695,0.0855168418978295,
0.412827461139898));
#16245=CARTESIAN_POINT('Ctrl Pts',(-0.0122846228212416,0.13866410438033,
0.420766450777203));
#16246=CARTESIAN_POINT('Ctrl Pts',(-0.123166656044517,0.0648738825743514,
0.428705440414509));
#16247=CARTESIAN_POINT('Ctrl Pts',(-0.121298056821252,-0.0683039326309071,
0.436644430051815));
#16248=CARTESIAN_POINT('Ctrl Pts',(-0.00838939967687663,-0.138954178686792,
0.44458341968912));
#16249=CARTESIAN_POINT('Ctrl Pts',(0.11219917790857,-0.0824013973067221,
0.452522409326426));
#16250=CARTESIAN_POINT('Ctrl Pts',(0.13007709763057,0.0495842159710775,
0.460461398963732));
#16251=CARTESIAN_POINT('Ctrl Pts',(0.0288783492374893,0.136178877755608,
0.468400388601037));
#16252=CARTESIAN_POINT('Ctrl Pts',(-0.0987565487199846,0.0981111099028881,
0.476339378238344));
#16253=CARTESIAN_POINT('Ctrl Pts',(-0.135986594552616,-0.0297706550724338,
0.484278367875649));
#16254=CARTESIAN_POINT('Ctrl Pts',(-0.0487302328423073,-0.130399425645183,
0.492217357512954));
#16255=CARTESIAN_POINT('Ctrl Pts',(0.0831353173341669,-0.111656458896056,
0.50015634715026));
#16256=CARTESIAN_POINT('Ctrl Pts',(0.13889618212661,0.00930034365552528,
0.508095336787567));
#16257=CARTESIAN_POINT('Ctrl Pts',(0.0675071113591811,0.12174331898465,
0.516034326424871));
#16258=CARTESIAN_POINT('Ctrl Pts',(-0.0656800932930844,0.122738629397884,
0.523973316062178));
#16259=CARTESIAN_POINT('Ctrl Pts',(-0.138741673886299,0.0113751364249866,
0.531912305699483));
#16260=CARTESIAN_POINT('Ctrl Pts',(-0.0847947606245053,-0.110401514355972,
0.539851295336789));
#16261=CARTESIAN_POINT('Ctrl Pts',(0.0467759446245483,-0.131113145053959,
0.547790284974095));
#16262=CARTESIAN_POINT('Ctrl Pts',(0.135526478334676,-0.031799677225719,
0.555729274611401));
#16263=CARTESIAN_POINT('Ctrl Pts',(0.100211809365564,0.0966242157284558,
0.563668264248707));
#16264=CARTESIAN_POINT('Ctrl Pts',(-0.0268399031138932,0.136595261273209,
0.571607253886012));
#16265=CARTESIAN_POINT('Ctrl Pts',(-0.129321523751272,0.0515227066069736,
0.579546243523318));
#16266=CARTESIAN_POINT('Ctrl Pts',(-0.113418152377209,-0.0807153548762533,
0.587485233160623));
#16267=CARTESIAN_POINT('Ctrl Pts',(0.00631176444456456,-0.139064040754811,
0.595424222797929));
#16268=CARTESIAN_POINT('Ctrl Pts',(0.120263693490807,-0.0701091280034811,
0.603363212435234));
#16269=CARTESIAN_POINT('Ctrl Pts',(0.124122453355413,0.0630258865426945,
0.611302202072541));
#16270=CARTESIAN_POINT('Ctrl Pts',(0.0143556138404206,0.138465021405133,
0.619241191709845));
#16271=CARTESIAN_POINT('Ctrl Pts',(-0.108552806291007,0.0871489187988374,
0.627180181347153));
#16272=CARTESIAN_POINT('Ctrl Pts',(-0.132088571872698,-0.043946046262323,
0.635119170984457));
#16273=CARTESIAN_POINT('Ctrl Pts',(-0.0347063025259737,-0.134811417789573,
0.643058160621763));
#16274=CARTESIAN_POINT('Ctrl Pts',(0.0944472082050275,-0.102266175560326,
0.65099715025907));
#16275=CARTESIAN_POINT('Ctrl Pts',(0.137140772714236,0.0238967416356601,
0.658936139896373));
#16276=CARTESIAN_POINT('Ctrl Pts',(0.054291358674537,0.128183829614862,
0.666875129533682));
#16277=CARTESIAN_POINT('Ctrl Pts',(-0.0782580734018908,0.115127406593233,
0.674814119170985));
#16278=CARTESIAN_POINT('Ctrl Pts',(-0.139167602654929,-0.00332026696803425,
0.682753108808293));
#16279=CARTESIAN_POINT('Ctrl Pts',(-0.0726787294560835,-0.118728463672822,
0.690692098445597));
#16280=CARTESIAN_POINT('Ctrl Pts',(0.0603425395611779,-0.125448888878168,
0.698631088082904));
#16281=CARTESIAN_POINT('Ctrl Pts',(0.138124349154501,-0.0173294538893964,
0.706570077720209));
#16282=CARTESIAN_POINT('Ctrl Pts',(0.0894627833767505,0.106653908470079,
0.714509067357515));
#16283=CARTESIAN_POINT('Ctrl Pts',(-0.0410958292974484,0.133002927094911,
0.72244805699482));
#16284=CARTESIAN_POINT('Ctrl Pts',(-0.134034026730954,0.0375968812502473,
0.730387046632127));
#16285=CARTESIAN_POINT('Ctrl Pts',(-0.104273258644039,-0.0922265326964679,
0.738326036269432));
#16286=CARTESIAN_POINT('Ctrl Pts',(0.0209425314183671,-0.137622876656644,
0.746265025906738));
#16287=CARTESIAN_POINT('Ctrl Pts',(0.126986869252672,-0.0570349089493802,
0.754204015544043));
#16288=CARTESIAN_POINT('Ctrl Pts',(0.11678343126468,0.0757646090434518,
0.762143005181349));
#16289=CARTESIAN_POINT('Ctrl Pts',(-0.000327234354877375,0.139206819944772,
0.770081994818654));
#16290=CARTESIAN_POINT('Ctrl Pts',(-0.117138339349379,0.0752147276530931,
0.778020984455961));
#16291=CARTESIAN_POINT('Ctrl Pts',(-0.126717322684213,-0.0576312930030564,
0.785959974093266));
#16292=CARTESIAN_POINT('Ctrl Pts',(-0.0202952816069424,-0.137719814645367,
0.793898963730571));
#16293=CARTESIAN_POINT('Ctrl Pts',(0.104705698854998,-0.0917352845351548,
0.801837953367879));
#16294=CARTESIAN_POINT('Ctrl Pts',(0.133855787965376,0.0382266115373486,
0.809776943005182));
#16295=CARTESIAN_POINT('Ctrl Pts',(0.0404700769297216,0.133194664588195,
0.81771593264249));
#16296=CARTESIAN_POINT('Ctrl Pts',(-0.0899632159395838,0.106232130635072,
0.825654922279794));
#16297=CARTESIAN_POINT('Ctrl Pts',(-0.13804135019805,-0.0179786383510676,
0.833593911917101));
#16298=CARTESIAN_POINT('Ctrl Pts',(-0.059752088941783,-0.125731196083361,
0.841532901554406));
#16299=CARTESIAN_POINT('Ctrl Pts',(0.0732361146625898,-0.118385460722959,
0.849471891191712));
#16300=CARTESIAN_POINT('Ctrl Pts',(0.139181674492094,-0.00266594955618734,
0.857410880829018));
#16301=CARTESIAN_POINT('Ctrl Pts',(0.077715950067195,0.115494055719818,
0.865349870466323));
#16302=CARTESIAN_POINT('Ctrl Pts',(-0.0548934004223171,0.127927168308903,
0.87328886010363));
#16303=CARTESIAN_POINT('Ctrl Pts',(-0.137251604915624,0.0232517257326144,
0.881227849740934));
#16304=CARTESIAN_POINT('Ctrl Pts',(-0.0939653715754795,-0.102709078207047,
0.889166839378241));
#16305=CARTESIAN_POINT('Ctrl Pts',(0.0353397195745277,-0.134646760160997,
0.897105829015547));
#16306=CARTESIAN_POINT('Ctrl Pts',(0.132293719443212,-0.0433245611326863,
0.905044818652852));
#16307=CARTESIAN_POINT('Ctrl Pts',(0.108141885842356,0.0876583043865096,
0.912983808290157));
#16308=CARTESIAN_POINT('Ctrl Pts',(-0.0150064327997127,0.138395999855801,
0.920922797927463));
#16309=CARTESIAN_POINT('Ctrl Pts',(-0.124417390671652,0.0624416423544169,
0.928861787564769));
#16310=CARTESIAN_POINT('Ctrl Pts',(-0.119932754264349,-0.0706737593172073,
0.936800777202075));
#16311=CARTESIAN_POINT('Ctrl Pts',(-0.00565790085648466,-0.139092177922979,
0.944739766839381));
#16312=CARTESIAN_POINT('Ctrl Pts',(0.113796373024222,-0.0801812402497705,
0.952678756476687));
#16313=CARTESIAN_POINT('Ctrl Pts',(0.129077866376032,0.0521301276928276,
0.960617746113992));
#16314=CARTESIAN_POINT('Ctrl Pts',(0.026197419344502,0.13671993644362,0.968556735751298));
#16315=CARTESIAN_POINT('Ctrl Pts',(-0.100664969670515,0.0961520134094621,
0.976495725388603));
#16316=CARTESIAN_POINT('Ctrl Pts',(-0.13537547797311,-0.0324364881732178,
0.98443471502591));
#16317=CARTESIAN_POINT('Ctrl Pts',(-0.0461590140787468,-0.131331607851033,
0.992373704663214));
#16318=CARTESIAN_POINT('Ctrl Pts',(0.0853128637208732,-0.110001641284132,
1.00031269430052));
#16319=CARTESIAN_POINT('Ctrl Pts',(0.138686661656432,0.0120272889735618,
1.00825168393783));
#16320=CARTESIAN_POINT('Ctrl Pts',(0.0651023256631918,0.123046060459907,
1.01619067357513));
#16321=CARTESIAN_POINT('Ctrl Pts',(-0.0680787277209358,0.121424596492465,
1.02412966321244));
#16322=CARTESIAN_POINT('Ctrl Pts',(-0.138938371616466,0.00864723620724691,
1.03206865284975));
#16323=CARTESIAN_POINT('Ctrl Pts',(-0.0826094583655966,-0.112046076191904,
1.04000764248705));
#16324=CARTESIAN_POINT('Ctrl Pts',(0.0493427524230464,-0.130168884856471,
1.04794663212436));
#16325=CARTESIAN_POINT('Ctrl Pts',(0.136125055048066,-0.0291310004912345,
1.05588562176166));
#16326=CARTESIAN_POINT('Ctrl Pts',(0.0982941990358779,0.0985743183458784,
1.06382461139897));
#16327=CARTESIAN_POINT('Ctrl Pts',(-0.0295182596522469,0.136041604476578,
1.07176360103627));
#16328=CARTESIAN_POINT('Ctrl Pts',(-0.130308774647192,0.0489721252490281,
1.07970259067358));
#16329=CARTESIAN_POINT('Ctrl Pts',(-0.111810537096203,-0.0829279783650712,
1.08764158031088));
#16330=CARTESIAN_POINT('Ctrl Pts',(0.00904258428980543,-0.13891320121148,
1.09558056994819));
#16331=CARTESIAN_POINT('Ctrl Pts',(0.121617839487272,-0.067732908692211,
1.1035195595855));
#16332=CARTESIAN_POINT('Ctrl Pts',(0.122860297649024,0.0654522196953821,
1.1114585492228));
#16333=CARTESIAN_POINT('Ctrl Pts',(0.0116325734791967,0.138720326685422,
1.11939753886011));
#16334=CARTESIAN_POINT('Ctrl Pts',(-0.110243974478508,0.0849994817198388,
1.12733652849741));
#16335=CARTESIAN_POINT('Ctrl Pts',(-0.131199719314147,-0.0465325633653302,
1.13527551813472));
#16336=CARTESIAN_POINT('Ctrl Pts',(-0.0320511128216771,-0.13546723577438,
1.14321450777202));
#16337=CARTESIAN_POINT('Ctrl Pts',(0.0964380908528195,-0.100390938007982,
1.15115349740933));
#16338=CARTESIAN_POINT('Ctrl Pts',(0.136644831685568,0.0265863832644056,
1.15909248704664));
#16339=CARTESIAN_POINT('Ctrl Pts',(0.0517625939920979,0.129225692742072,
1.16703147668394));
#16340=CARTESIAN_POINT('Ctrl Pts',(-0.0805047509788913,0.113567736929491,
1.17497046632125));
#16341=CARTESIAN_POINT('Ctrl Pts',(-0.139075513779617,-0.00605369873671642,
1.18290945595855));
#16342=CARTESIAN_POINT('Ctrl Pts',(-0.0703321751825429,-0.12013338809653,
1.19084844559586));
#16343=CARTESIAN_POINT('Ctrl Pts',(0.0627954496153871,-0.124239193932754,
1.19878743523316));
#16344=CARTESIAN_POINT('Ctrl Pts',(0.138438143943654,-0.0146125323915816,
1.20672642487047));
#16345=CARTESIAN_POINT('Ctrl Pts',(0.0873502052771435,0.108390901091839,
1.21466541450777));
#16346=CARTESIAN_POINT('Ctrl Pts',(-0.043700859820065,0.132169893139269,
1.22260440414508));
#16347=CARTESIAN_POINT('Ctrl Pts',(-0.134746782767514,0.0349564062120582,
1.23054339378239));
#16348=CARTESIAN_POINT('Ctrl Pts',(-0.102441260891455,-0.0942572748833364,
1.23848238341969));
#16349=CARTESIAN_POINT('Ctrl Pts',(0.0236422145726536,-0.137184880695923,
1.246421373057));
#16350=CARTESIAN_POINT('Ctrl Pts',(0.128082862902196,-0.0545291301253663,
1.2543603626943));
#16351=CARTESIAN_POINT('Ctrl Pts',(0.115272428336817,0.0780443019497631,
1.26229935233161));
#16352=CARTESIAN_POINT('Ctrl Pts',(-0.00306201423577413,0.139173524314926,
1.27023834196891));
#16353=CARTESIAN_POINT('Ctrl Pts',(-0.118593392628464,0.0728989233548558,
1.27817733160622));
#16354=CARTESIAN_POINT('Ctrl Pts',(-0.125560647806918,-0.06010964584811,
1.28611632124353));
#16355=CARTESIAN_POINT('Ctrl Pts',(-0.0175857351491984,-0.138091953858251,
1.29405531088083));
#16356=CARTESIAN_POINT('Ctrl Pts',(0.106487712804436,-0.089660542174548,
1.30199430051814));
#16357=CARTESIAN_POINT('Ctrl Pts',(0.133078957772855,0.0408489510387311,
1.30993329015544));
#16358=CARTESIAN_POINT('Ctrl Pts',(0.0378455373822902,0.133964029124136,
1.31787227979275));
#16359=CARTESIAN_POINT('Ctrl Pts',(-0.0920328787300654,0.104444219726284,
1.32581126943006));
#16360=CARTESIAN_POINT('Ctrl Pts',(-0.137661501842601,-0.0206871148492911,
1.33375025906736));
#16361=CARTESIAN_POINT('Ctrl Pts',(-0.0572704544775333,-0.126880813469472,
1.34168924870467));
#16362=CARTESIAN_POINT('Ctrl Pts',(0.0755477687720905,-0.116923823242002,
1.34962823834197));
#16363=CARTESIAN_POINT('Ctrl Pts',(0.13920718769651,6.89141801743488E-5,
1.35756722797928));
#16364=CARTESIAN_POINT('Ctrl Pts',(0.0754319660950179,0.116998564767658,
1.36550621761658));
#16365=CARTESIAN_POINT('Ctrl Pts',(-0.0573960494825499,0.126824048933643,
1.37344520725389));
#16366=CARTESIAN_POINT('Ctrl Pts',(-0.13768191782304,0.0205508058651932,
1.38138419689119));
#16367=CARTESIAN_POINT('Ctrl Pts',(-0.0919294216917856,-0.104535287252199,
1.3893231865285));
#16368=CARTESIAN_POINT('Ctrl Pts',(0.0379781508110965,-0.133926497290667,
1.39726217616581));
#16369=CARTESIAN_POINT('Ctrl Pts',(0.133119345865688,-0.0407171622080862,
1.40520116580311));
#16370=CARTESIAN_POINT('Ctrl Pts',(0.106398871137127,0.0897659150453452,
1.41314015544042));
#16371=CARTESIAN_POINT('Ctrl Pts',(-0.0177224175491345,0.138074504763813,
1.42107914507772));
#16372=CARTESIAN_POINT('Ctrl Pts',(-0.125620162573399,0.0599852426217579,
1.42901813471503));
#16373=CARTESIAN_POINT('Ctrl Pts',(-0.118521039729242,-0.0730161975746823,
1.43695712435233));
#16374=CARTESIAN_POINT('Ctrl Pts',(-0.00292444232197888,-0.139176693688359,
1.44489611398964));
#16375=CARTESIAN_POINT('Ctrl Pts',(0.115350068603298,-0.0779297424218237,
1.45283510362695));
#16376=CARTESIAN_POINT('Ctrl Pts',(0.128028003046829,0.0546551750765237,
1.46077409326425));
#16377=CARTESIAN_POINT('Ctrl Pts',(0.0235079116789307,0.137209630484779,
1.46871308290156));
#16378=CARTESIAN_POINT('Ctrl Pts',(-0.102537447198224,0.0941531272373115,
1.47665207253886));
#16379=CARTESIAN_POINT('Ctrl Pts',(-0.134706575776555,-0.0350847218495708,
1.48459106217617));
#16380=CARTESIAN_POINT('Ctrl Pts',(-0.0435804807853106,-0.132222740314769,
1.49253005181348));
#16381=CARTESIAN_POINT('Ctrl Pts',(0.0874774386997331,-0.108286040948335,
1.50046904145078));
#16382=CARTESIAN_POINT('Ctrl Pts',(0.138385550162814,0.0147146982980264,
1.50840803108809));
#16383=CARTESIAN_POINT('Ctrl Pts',(0.0627460642121078,0.124368470664037,
1.51634702072539));
#16384=CARTESIAN_POINT('Ctrl Pts',(-0.0706026869052757,0.119928391791904,
1.5242860103627));
#16385=CARTESIAN_POINT('Ctrl Pts',(-0.116004137797729,0.0441355889673283,
1.5295786701209));
#16386=CARTESIAN_POINT('Ctrl Pts',(-0.117668597464313,0.00500517689812487,
1.532225));
#16387=CARTESIAN_POINT('',(0.0684664424539461,-0.0958295198918396,0.));
#16388=CARTESIAN_POINT('Ctrl Pts',(0.0684664424539414,-0.095829519891843,
-1.38777878078145E-17));
#16389=CARTESIAN_POINT('Ctrl Pts',(0.100334321247169,-0.0730611673843044,
0.00264632987910189));
#16390=CARTESIAN_POINT('Ctrl Pts',(0.139021564822767,0.00636891437108143,
0.00793898963730573));
#16391=CARTESIAN_POINT('Ctrl Pts',(0.0699018669780613,0.120491966796142,
0.0158779792746114));
#16392=CARTESIAN_POINT('Ctrl Pts',(-0.0632645460347191,0.123954346655885,
0.0238169689119172));
#16393=CARTESIAN_POINT('Ctrl Pts',(-0.11596266760442,0.0470121293552651,
0.0293787386625077));
#16394=CARTESIAN_POINT('Ctrl Pts',(-0.117944740497024,0.00404481602818191,
0.0322941785339964));
#16395=CARTESIAN_POINT('Ctrl Pts',(-0.117917485785546,7.60014832213644E-5,
0.0325632885263832));
#16396=CARTESIAN_POINT('Ctrl Pts',(0.0635546915223951,0.132092229195826,
-2.16840434497101E-19));
#16397=CARTESIAN_POINT('Ctrl Pts',(0.0668114782730532,0.13015255741457,
-1.00603861447787E-18));
#16398=CARTESIAN_POINT('Ctrl Pts',(0.0699821360194518,0.12808121947321,
-2.9262196004085E-17));
#16399=CARTESIAN_POINT('Ctrl Pts',(0.0730575207853233,0.125877721325919,
-2.71050543121376E-17));
#16400=CARTESIAN_POINT('Ctrl Pts',(0.0789281193465506,0.121671466161783,
-2.36378102375718E-17));
#16401=CARTESIAN_POINT('Ctrl Pts',(0.0844522091809674,0.11698398814956,
1.43782932504085E-18));
#16402=CARTESIAN_POINT('Ctrl Pts',(0.0895990070394484,0.111875963994554,
9.97465998686664E-18));
#16403=CARTESIAN_POINT('Ctrl Pts',(0.0928865546640729,0.108613183302742,
1.54276111490851E-17));
#16404=CARTESIAN_POINT('Ctrl Pts',(0.0960206821069302,0.105176950779614,
-2.53636710091701E-17));
#16405=CARTESIAN_POINT('Ctrl Pts',(0.098978417360439,0.101599719103904,
-1.56125112837913E-17));
#16406=CARTESIAN_POINT('Ctrl Pts',(0.103148772110026,0.0965558852815647,
-1.86354736740503E-18));
#16407=CARTESIAN_POINT('Ctrl Pts',(0.106976174326278,0.0912251680483688,
1.1337629845105E-17));
#16408=CARTESIAN_POINT('Ctrl Pts',(0.110435561611279,0.0856523061447448,
2.03830008427275E-17));
#16409=CARTESIAN_POINT('Ctrl Pts',(0.112407683932559,0.0824753373788608,
2.55395723911076E-17));
#16410=CARTESIAN_POINT('Ctrl Pts',(0.114261188142284,0.0792174064057451,
2.29308760465575E-17));
#16411=CARTESIAN_POINT('Ctrl Pts',(0.115986535786665,0.0758936579718971,
2.08166817117217E-17));
#16412=CARTESIAN_POINT('Ctrl Pts',(0.120573220307724,0.0670577659456877,
1.51962825639422E-17));
#16413=CARTESIAN_POINT('Ctrl Pts',(0.124235263225439,0.0578042025119142,
2.52358375750583E-18));
#16414=CARTESIAN_POINT('Ctrl Pts',(0.126883306113679,0.0482911783993335,
1.30104260698261E-17));
#16415=CARTESIAN_POINT('Ctrl Pts',(0.128478610866444,0.0425600882242624,
1.93281898253259E-17));
#16416=CARTESIAN_POINT('Ctrl Pts',(0.129704960854084,0.0367345196138549,
-5.78096029915021E-19));
#16417=CARTESIAN_POINT('Ctrl Pts',(0.130533291754837,0.0308494671050701,
0.));
#16418=CARTESIAN_POINT('Ctrl Pts',(0.131003715791213,0.0275072397983871,
3.2831114661813E-19));
#16419=CARTESIAN_POINT('Ctrl Pts',(0.131345346899704,0.0241444941465381,
-1.7128612844445E-18));
#16420=CARTESIAN_POINT('Ctrl Pts',(0.131551728167405,0.0207857616715298,
2.60208521396521E-18));
#16421=CARTESIAN_POINT('Ctrl Pts',(0.131851321606701,0.0159100565018035,
8.86587880453295E-18));
#16422=CARTESIAN_POINT('Ctrl Pts',(0.131867617692795,0.0110341713389591,
-1.68111772803455E-17));
#16423=CARTESIAN_POINT('Ctrl Pts',(0.131586936334964,0.0061777758930637,
-6.93889390390723E-18));
#16424=CARTESIAN_POINT('Ctrl Pts',(0.131099036368572,-0.00226395031615145,
9.98510028643051E-18));
#16425=CARTESIAN_POINT('Ctrl Pts',(0.129715139118287,-0.0106479390144509,
1.03491660509995E-17));
#16426=CARTESIAN_POINT('Ctrl Pts',(0.127493709984164,-0.018859987399606,
1.04083408558608E-17));
#16427=CARTESIAN_POINT('Ctrl Pts',(0.126553994220251,-0.0223338732882013,
1.04333731632617E-17));
#16428=CARTESIAN_POINT('Ctrl Pts',(0.125463061762623,-0.0257782540966497,
1.75224609115742E-17));
#16429=CARTESIAN_POINT('Ctrl Pts',(0.124232565886791,-0.0291638780753137,
1.73472347597681E-17));
#16430=CARTESIAN_POINT('Ctrl Pts',(0.12170396813588,-0.0361211392462112,
1.69871551674183E-17));
#16431=CARTESIAN_POINT('Ctrl Pts',(0.118582485980247,-0.0428512226170345,
-6.45748389186585E-19));
#16432=CARTESIAN_POINT('Ctrl Pts',(0.114911168983798,-0.0492778939609075,
3.46944695195361E-18));
#16433=CARTESIAN_POINT('Ctrl Pts',(0.112347970921096,-0.0537647937721124,
6.34254691478841E-18));
#16434=CARTESIAN_POINT('Ctrl Pts',(0.109516356061708,-0.0581036184196785,
-1.05628593522785E-17));
#16435=CARTESIAN_POINT('Ctrl Pts',(0.106427098863261,-0.0622637901458048,
-1.21430643318376E-17));
#16436=CARTESIAN_POINT('Ctrl Pts',(0.104287070791936,-0.0651456752410043,
-1.32377232732828E-17));
#16437=CARTESIAN_POINT('Ctrl Pts',(0.102021590876101,-0.067943056099314,
-1.03088264066386E-17));
#16438=CARTESIAN_POINT('Ctrl Pts',(0.0996491962474235,-0.0706287444932102,
-1.04083408558608E-17));
#16439=CARTESIAN_POINT('Ctrl Pts',(0.0938611946766418,-0.0771810981592459,
-1.06511292104842E-17));
#16440=CARTESIAN_POINT('Ctrl Pts',(0.0874218747326319,-0.0830961188460978,
9.460259835177E-18));
#16441=CARTESIAN_POINT('Ctrl Pts',(0.0803902102994179,-0.0882260767030795,
2.94902990916057E-17));
#16442=CARTESIAN_POINT('Ctrl Pts',(0.0765868618375105,-0.091000813397402,
4.03243227742548E-17));
#16443=CARTESIAN_POINT('Ctrl Pts',(0.0726097989303321,-0.0935451549285004,
-2.49510848448888E-18));
#16444=CARTESIAN_POINT('Ctrl Pts',(0.0684664424539416,-0.0958295198918429,
0.));
#16445=CARTESIAN_POINT('Ctrl Pts',(-0.00156962371674571,0.146072546381438,
1.50365));
#16446=CARTESIAN_POINT('Ctrl Pts',(0.0218361081466035,0.146362061217761,
1.50238307892777));
#16447=CARTESIAN_POINT('Ctrl Pts',(0.0452966847593804,0.141345883428421,
1.50111615785553));
#16448=CARTESIAN_POINT('Ctrl Pts',(0.0660179268768178,0.130913916311315,
1.4998492367833));
#16449=CARTESIAN_POINT('Ctrl Pts',(0.109300214423576,0.109123745727819,
1.4972029069042));
#16450=CARTESIAN_POINT('Ctrl Pts',(0.140630685714559,0.0637042888941242,
1.49455657702509));
#16451=CARTESIAN_POINT('Ctrl Pts',(0.145752650840527,0.0155206226173656,
1.49191024714599));
#16452=CARTESIAN_POINT('Ctrl Pts',(0.150874615966495,-0.0326630436593903,
1.48926391726689));
#16453=CARTESIAN_POINT('Ctrl Pts',(0.129788074927449,-0.0836109193792113,
1.48661758738779));
#16454=CARTESIAN_POINT('Ctrl Pts',(0.0921021927661857,-0.114042242015571,
1.48397125750869));
#16455=CARTESIAN_POINT('Ctrl Pts',(0.0544163106049216,-0.144473564651931,
1.48132492762959));
#16456=CARTESIAN_POINT('Ctrl Pts',(0.000131087321441313,-0.154388334204831,
1.47867859775048));
#16457=CARTESIAN_POINT('Ctrl Pts',(-0.0458840977328367,-0.139228052523514,
1.47603226787138));
#16458=CARTESIAN_POINT('Ctrl Pts',(-0.0918992827871148,-0.124067770842196,
1.47338593799228));
#16459=CARTESIAN_POINT('Ctrl Pts',(-0.129644429612189,-0.0838324379266627,
1.47073960811318));
#16460=CARTESIAN_POINT('Ctrl Pts',(-0.141854649713415,-0.0369491035797489,
1.46809327823408));
#16461=CARTESIAN_POINT('Ctrl Pts',(-0.14497337938942,-0.0249741805295802,
1.46741735368415));
#16462=CARTESIAN_POINT('Ctrl Pts',(-0.146426231435716,-0.0125655473306973,
1.46674142913422));
#16463=CARTESIAN_POINT('Ctrl Pts',(-0.14631473222987,-0.000131398079681141,
1.46606550458429));
#16464=CARTESIAN_POINT('Origin',(0.,0.,-0.0924367114736175));
#16465=CARTESIAN_POINT('',(-0.0684664424539507,-0.0958295198918364,0.));
#16466=CARTESIAN_POINT('Ctrl Pts',(-0.0686146973663072,-0.0959584553529141,
8.16675286424706E-17));
#16467=CARTESIAN_POINT('Ctrl Pts',(-0.0391968190522335,-0.116741470120209,
0.00244290680874874));
#16468=CARTESIAN_POINT('Ctrl Pts',(0.0436301113039178,-0.130476273073809,
0.0075332029917574));
#16469=CARTESIAN_POINT('Ctrl Pts',(0.134092250525203,-0.0374520209666004,
0.0152708885490261));
#16470=CARTESIAN_POINT('Ctrl Pts',(0.104134301645602,0.0924305194826295,
0.023213056671806));
#16471=CARTESIAN_POINT('Ctrl Pts',(-0.0212379681243542,0.137589894578696,
0.0311552247945861));
#16472=CARTESIAN_POINT('Ctrl Pts',(-0.106685947947232,0.0723488109778776,
0.0375631097285225));
#16473=CARTESIAN_POINT('Ctrl Pts',(-0.117663533972591,0.0165813593984342,
0.041323605288199));
#16474=CARTESIAN_POINT('Ctrl Pts',(-0.117600989619072,5.04992496179954E-5,
0.0424367114736154));
#16475=CARTESIAN_POINT('Origin',(0.,0.,0.));
#16476=CARTESIAN_POINT('Ctrl Pts',(-0.0510216505388318,0.106149619882943,
-0.0164977839420939));
#16477=CARTESIAN_POINT('Ctrl Pts',(-0.0863355867949722,0.0891756983861136,
-0.0138503945678339));
#16478=CARTESIAN_POINT('Ctrl Pts',(-0.13808023131828,0.0175094743621551,
-0.00855561581931395));
#16479=CARTESIAN_POINT('Ctrl Pts',(-0.0894531427980795,-0.106808298616542,
-0.000613447696533924));
#16480=CARTESIAN_POINT('Ctrl Pts',(0.0412394829729132,-0.132934609947913,
0.00732872042624606));
#16481=CARTESIAN_POINT('Ctrl Pts',(0.134092250525203,-0.0374520209666004,
0.0152708885490261));
#16482=CARTESIAN_POINT('Ctrl Pts',(0.104134301645602,0.0924305194826295,
0.023213056671806));
#16483=CARTESIAN_POINT('Ctrl Pts',(-0.0212379681243542,0.137589894578696,
0.0311552247945861));
#16484=CARTESIAN_POINT('Ctrl Pts',(-0.127145335141994,0.0567276974868182,
0.039097392917366));
#16485=CARTESIAN_POINT('Ctrl Pts',(-0.116579117211717,-0.0761160149501382,
0.0470395610401461));
#16486=CARTESIAN_POINT('Ctrl Pts',(0.000787973702835166,-0.139222729671589,
0.054981729162926));
#16487=CARTESIAN_POINT('Ctrl Pts',(0.117431922513572,-0.0747907597173192,
0.0629238972857061));
#16488=CARTESIAN_POINT('Ctrl Pts',(0.126496838785129,0.0581591461343325,
0.070866065408486));
#16489=CARTESIAN_POINT('Ctrl Pts',(0.0196773008918215,0.137828289815661,
0.0788082335312661));
#16490=CARTESIAN_POINT('Ctrl Pts',(-0.105168479521776,0.0912330920368172,
0.0867504016540459));
#16491=CARTESIAN_POINT('Ctrl Pts',(-0.133669226619255,-0.0389412707994331,
0.0946925697768262));
#16492=CARTESIAN_POINT('Ctrl Pts',(-0.0397151780004399,-0.133441281507892,
0.102634737899606));
#16493=CARTESIAN_POINT('Ctrl Pts',(0.0906220264938673,-0.105695447092796,
0.110576906022386));
#16494=CARTESIAN_POINT('Ctrl Pts',(0.137940159127448,0.0188783162799928,
0.118519074145166));
#16495=CARTESIAN_POINT('Ctrl Pts',(0.0588909273047484,0.126157580947307,
0.126461242267946));
#16496=CARTESIAN_POINT('Ctrl Pts',(-0.074108440039672,0.117863552156501,
0.134403410390726));
#16497=CARTESIAN_POINT('Ctrl Pts',(-0.139216864956951,0.00159439502933392,
0.142345578513506));
#16498=CARTESIAN_POINT('Ctrl Pts',(-0.0767883381764272,-0.116135388594389,
0.150287746636286));
#16499=CARTESIAN_POINT('Ctrl Pts',(0.0559861945572589,-0.127473226882309,
0.158229914759066));
#16500=CARTESIAN_POINT('Ctrl Pts',(0.137471621702818,-0.0220324926503626,
0.166172082881846));
#16501=CARTESIAN_POINT('Ctrl Pts',(0.0930189202108026,0.103592267873211,
0.174114251004626));
#16502=CARTESIAN_POINT('Ctrl Pts',(-0.0366486683060043,0.134315868829211,
0.182056419127406));
#16503=CARTESIAN_POINT('Ctrl Pts',(-0.132742311638566,0.0419923350165386,
0.189998587250186));
#16504=CARTESIAN_POINT('Ctrl Pts',(-0.107230360350792,-0.0888004916405464,
0.197940755372966));
#16505=CARTESIAN_POINT('Ctrl Pts',(0.0165156171993534,-0.138242945169174,
0.205882923495746));
#16506=CARTESIAN_POINT('Ctrl Pts',(0.125131592687617,-0.061040658666823,
0.213825091618526));
#16507=CARTESIAN_POINT('Ctrl Pts',(0.119114174013628,0.0720811421096423,
0.221767259741306));
#16508=CARTESIAN_POINT('Ctrl Pts',(0.0039759348809324,0.139169211541763,
0.229709427864086));
#16509=CARTESIAN_POINT('Ctrl Pts',(-0.114804669066963,0.0787639858025777,
0.237651595986866));
#16510=CARTESIAN_POINT('Ctrl Pts',(-0.128412401817242,-0.0537971426620367,
0.245593764109646));
#16511=CARTESIAN_POINT('Ctrl Pts',(-0.024381182195918,-0.137074561658528,
0.253535932232426));
#16512=CARTESIAN_POINT('Ctrl Pts',(0.101985705091022,-0.094777599970642,
0.261478100355206));
#16513=CARTESIAN_POINT('Ctrl Pts',(0.134923209124943,0.0343453801629359,
0.269420268477986));
#16514=CARTESIAN_POINT('Ctrl Pts',(0.0442571924125319,0.132004463632409,
0.277362436600766));
#16515=CARTESIAN_POINT('Ctrl Pts',(-0.0869529592639067,0.108733897080731,
0.285304604723546));
#16516=CARTESIAN_POINT('Ctrl Pts',(-0.138505267237684,-0.0141480898545381,
0.293246772846326));
#16517=CARTESIAN_POINT('Ctrl Pts',(-0.0631725212350128,-0.124068972994571,
0.301188940969106));
#16518=CARTESIAN_POINT('Ctrl Pts',(0.0700327441786229,-0.12032993078169,
0.309131109091886));
#16519=CARTESIAN_POINT('Ctrl Pts',(0.139080821187468,-0.00635631000930847,
0.317073277214666));
#16520=CARTESIAN_POINT('Ctrl Pts',(0.0807165776729536,0.11344034374014,
0.325015445337446));
#16521=CARTESIAN_POINT('Ctrl Pts',(-0.0515923433190751,0.129313988454311,
0.332957613460226));
#16522=CARTESIAN_POINT('Ctrl Pts',(-0.136637377548019,0.026722734813544,
0.340899781583006));
#16523=CARTESIAN_POINT('Ctrl Pts',(-0.0965085366518414,-0.100349289247285,
0.348841949705786));
#16524=CARTESIAN_POINT('Ctrl Pts',(0.0320320385160992,-0.135491055083419,
0.356784117828566));
#16525=CARTESIAN_POINT('Ctrl Pts',(0.131227975626944,-0.0465090949381858,
0.364726285951346));
#16526=CARTESIAN_POINT('Ctrl Pts',(0.110205605501345,0.0850799742312894,
0.372668454074126));
#16527=CARTESIAN_POINT('Ctrl Pts',(-0.0117764211155082,0.138727046407055,
0.380610622196906));
#16528=CARTESIAN_POINT('Ctrl Pts',(-0.122970036152848,0.065285892102983,
0.388552790319686));
#16529=CARTESIAN_POINT('Ctrl Pts',(-0.121510464882371,-0.0679638464419502,
0.396494958442466));
#16530=CARTESIAN_POINT('Ctrl Pts',(-0.00873482453528946,-0.138951719454826,
0.404437126565246));
#16531=CARTESIAN_POINT('Ctrl Pts',(0.112042812448737,-0.0826455423945668,
0.412379294688026));
#16532=CARTESIAN_POINT('Ctrl Pts',(0.130177722634257,0.049372441998279,
0.420321462810806));
#16533=CARTESIAN_POINT('Ctrl Pts',(0.0290564652212241,0.136160197297018,
0.428263630933586));
#16534=CARTESIAN_POINT('Ctrl Pts',(-0.098683499418539,0.098211223603141,
0.436205799056366));
#16535=CARTESIAN_POINT('Ctrl Pts',(-0.136019240449831,-0.0297093205335648,
0.444147967179146));
#16536=CARTESIAN_POINT('Ctrl Pts',(-0.0487473834415776,-0.130413074907061,
0.452090135301926));
#16537=CARTESIAN_POINT('Ctrl Pts',(0.0831820848081396,-0.111645054821459,
0.460032303424706));
#16538=CARTESIAN_POINT('Ctrl Pts',(0.138908217753341,0.00940130521287039,
0.467974471547486));
#16539=CARTESIAN_POINT('Ctrl Pts',(0.0673801526530663,0.121835103839429,
0.475916639670265));
#16540=CARTESIAN_POINT('Ctrl Pts',(-0.0658750545035054,0.12265543075329,
0.483858807793047));
#16541=CARTESIAN_POINT('Ctrl Pts',(-0.138781944133385,0.0111107822259715,
0.491800975915825));
#16542=CARTESIAN_POINT('Ctrl Pts',(-0.084550315326251,-0.110612484274364,
0.499743144038607));
#16543=CARTESIAN_POINT('Ctrl Pts',(0.0471380885036503,-0.131003351527116,
0.507685312161385));
#16544=CARTESIAN_POINT('Ctrl Pts',(0.135643160584381,-0.031381690295376,
0.515627480284167));
#16545=CARTESIAN_POINT('Ctrl Pts',(0.0998851624184703,0.0969888232104648,
0.523569648406945));
#16546=CARTESIAN_POINT('Ctrl Pts',(-0.0273779061153799,0.136507610615132,
0.531511816529727));
#16547=CARTESIAN_POINT('Ctrl Pts',(-0.129560000008381,0.0509714027366644,
0.539453984652505));
#16548=CARTESIAN_POINT('Ctrl Pts',(-0.113051823689188,-0.0812598465397498,
0.547396152775286));
#16549=CARTESIAN_POINT('Ctrl Pts',(0.00702343738442799,-0.139048728244533,
0.555338320898066));
#16550=CARTESIAN_POINT('Ctrl Pts',(0.12066450826877,-0.0694546898587181,
0.563280489020846));
#16551=CARTESIAN_POINT('Ctrl Pts',(0.123764493242992,0.063766979789076,
0.571222657143626));
#16552=CARTESIAN_POINT('Ctrl Pts',(0.0134834875971477,0.13857154491934,
0.579164825266405));
#16553=CARTESIAN_POINT('Ctrl Pts',(-0.109149777898995,0.0864303389077871,
0.587106993389186));
#16554=CARTESIAN_POINT('Ctrl Pts',(-0.131790633456927,-0.0448899368693808,
0.595049161511966));
#16555=CARTESIAN_POINT('Ctrl Pts',(-0.0336977294021144,-0.135086418755761,
0.602991329634746));
#16556=CARTESIAN_POINT('Ctrl Pts',(0.0952657566843092,-0.101529863106778,
0.610933497757526));
#16557=CARTESIAN_POINT('Ctrl Pts',(0.136956022624868,0.025038477707157,
0.618875665880307));
#16558=CARTESIAN_POINT('Ctrl Pts',(0.0531805018142573,0.128669000640787,
0.626817834003085));
#16559=CARTESIAN_POINT('Ctrl Pts',(-0.0793138220987445,0.114425500318782,
0.634760002125867));
#16560=CARTESIAN_POINT('Ctrl Pts',(-0.139148536750765,-0.00464351367351466,
0.642702170248646));
#16561=CARTESIAN_POINT('Ctrl Pts',(-0.0715088964667609,-0.119458592094588,
0.650644338371427));
#16562=CARTESIAN_POINT('Ctrl Pts',(0.0616402393688536,-0.124837327709565,
0.658586506494205));
#16563=CARTESIAN_POINT('Ctrl Pts',(0.138320583400205,-0.0158522461166236,
0.666528674616987));
#16564=CARTESIAN_POINT('Ctrl Pts',(0.0882850628235238,0.107655121482266,
0.674470842739765));
#16565=CARTESIAN_POINT('Ctrl Pts',(-0.0426286451686149,0.132539337972556,
0.682413010862546));
#16566=CARTESIAN_POINT('Ctrl Pts',(-0.13449013477919,0.0360039045964495,
0.690355178985326));
#16567=CARTESIAN_POINT('Ctrl Pts',(-0.103144844235522,-0.0935148042116587,
0.698297347108106));
#16568=CARTESIAN_POINT('Ctrl Pts',(0.022691720100341,-0.137364345221032,
0.706239515230886));
#16569=CARTESIAN_POINT('Ctrl Pts',(0.127740337615313,-0.0553740340325759,
0.714181683353665));
#16570=CARTESIAN_POINT('Ctrl Pts',(0.115765682611161,0.077344581120379,
0.722123851476446));
#16571=CARTESIAN_POINT('Ctrl Pts',(-0.00226223072526165,0.139207614056346,
0.730066019599226));
#16572=CARTESIAN_POINT('Ctrl Pts',(-0.118217708309552,0.0735421711751344,
0.738008187722006));
#16573=CARTESIAN_POINT('Ctrl Pts',(-0.125873620115675,-0.059495455776806,
0.745950355844786));
#16574=CARTESIAN_POINT('Ctrl Pts',(-0.0182163644075178,-0.138029133036789,
0.753892523967566));
#16575=CARTESIAN_POINT('Ctrl Pts',(0.106128952536144,-0.0901139441634624,
0.761834692090347));
#16576=CARTESIAN_POINT('Ctrl Pts',(0.133249245915149,0.0403548753208232,
0.769776860213125));
#16577=CARTESIAN_POINT('Ctrl Pts',(0.0382995408207276,0.133854483197375,
0.777719028335907));
#16578=CARTESIAN_POINT('Ctrl Pts',(-0.0917364783268051,0.104729633071593,
0.785661196458685));
#16579=CARTESIAN_POINT('Ctrl Pts',(-0.137732458880487,-0.0203383202317681,
0.793603364581467));
#16580=CARTESIAN_POINT('Ctrl Pts',(-0.0575513573065257,-0.126774282767806,
0.801545532704245));
#16581=CARTESIAN_POINT('Ctrl Pts',(0.0753527000357912,-0.117071978271622,
0.809487700827026));
#16582=CARTESIAN_POINT('Ctrl Pts',(0.139225942868322,-0.000119714417332432,
0.817429868949805));
#16583=CARTESIAN_POINT('Ctrl Pts',(0.0755539188089132,0.116942220141962,
0.825372037072586));
#16584=CARTESIAN_POINT('Ctrl Pts',(-0.0573332568284509,0.12687306712048,
0.833314205195366));
#16585=CARTESIAN_POINT('Ctrl Pts',(-0.13769727914169,0.0205751504512258,
0.841256373318145));
#16586=CARTESIAN_POINT('Ctrl Pts',(-0.0919164475821765,-0.104571717796869,
0.849198541440926));
#16587=CARTESIAN_POINT('Ctrl Pts',(0.0380692928980519,-0.133920149482284,
0.857140709563706));
#16588=CARTESIAN_POINT('Ctrl Pts',(0.133179650076608,-0.0405839661022353,
0.865082877686486));
#16589=CARTESIAN_POINT('Ctrl Pts',(0.106283765719693,0.0899312995767124,
0.873025045809266));
#16590=CARTESIAN_POINT('Ctrl Pts',(-0.0179789669825735,0.138060255849953,
0.880967213932046));
#16591=CARTESIAN_POINT('Ctrl Pts',(-0.125771118879347,0.0597118342956578,
0.888909382054826));
#16592=CARTESIAN_POINT('Ctrl Pts',(-0.118344004924669,-0.0733387619032726,
0.896851550177606));
#16593=CARTESIAN_POINT('Ctrl Pts',(-0.00250162451743248,-0.139203517821528,
0.904793718300386));
#16594=CARTESIAN_POINT('Ctrl Pts',(0.115632500949424,-0.0775435504945224,
0.912735886423165));
#16595=CARTESIAN_POINT('Ctrl Pts',(0.127835376168433,0.0551542754370876,
0.920678054545947));
#16596=CARTESIAN_POINT('Ctrl Pts',(0.0229279137899797,0.137325118854324,
0.928620222668725));
#16597=CARTESIAN_POINT('Ctrl Pts',(-0.102983873094174,0.0936920454555137,
0.936562390791507));
#16598=CARTESIAN_POINT('Ctrl Pts',(-0.134551852288801,-0.0357725669300891,
0.944504558914285));
#16599=CARTESIAN_POINT('Ctrl Pts',(-0.0428565117498991,-0.132465832952297,
0.952446727037066));
#16600=CARTESIAN_POINT('Ctrl Pts',(0.0880997963686447,-0.107806787258123,
0.960388895159846));
#16601=CARTESIAN_POINT('Ctrl Pts',(0.138347640177547,0.0156143509765511,
0.968331063282625));
#16602=CARTESIAN_POINT('Ctrl Pts',(0.061854832590724,0.124731139593481,
0.976273231405407));
#16603=CARTESIAN_POINT('Ctrl Pts',(-0.0713033562375951,0.119581390225944,
0.984215399528185));
#16604=CARTESIAN_POINT('Ctrl Pts',(-0.139140345480169,0.00488280234845834,
0.992157567650966));
#16605=CARTESIAN_POINT('Ctrl Pts',(-0.0795104838321055,-0.114288934109561,
1.00009973577375));
#16606=CARTESIAN_POINT('Ctrl Pts',(0.0529591494285269,-0.128760265574912,
1.00804190389653));
#16607=CARTESIAN_POINT('Ctrl Pts',(0.136912761112491,-0.0252739657289669,
1.0159840720193));
#16608=CARTESIAN_POINT('Ctrl Pts',(0.0954402180350474,0.101365883217864,
1.02392624014209));
#16609=CARTESIAN_POINT('Ctrl Pts',(-0.0334653697086341,0.135144169424284,
1.03186840826486));
#16610=CARTESIAN_POINT('Ctrl Pts',(-0.131713240771149,0.0451165125500212,
1.03981057638765));
#16611=CARTESIAN_POINT('Ctrl Pts',(-0.109298251871946,-0.0862425048155002,
1.04775274451043));
#16612=CARTESIAN_POINT('Ctrl Pts',(0.0132451643780021,-0.13859452774087,
1.05569491263321));
#16613=CARTESIAN_POINT('Ctrl Pts',(0.123654649330263,-0.0639797248987874,
1.06363708075599));
#16614=CARTESIAN_POINT('Ctrl Pts',(0.120783771971213,0.0692470788374567,
1.07157924887876));
#16615=CARTESIAN_POINT('Ctrl Pts',(0.00726255089817806,0.139036444335888,
1.07952141700155));
#16616=CARTESIAN_POINT('Ctrl Pts',(-0.112911912907791,0.0814541430660127,
1.08746358512433));
#16617=CARTESIAN_POINT('Ctrl Pts',(-0.129647464608677,-0.0507485213543897,
1.09540575324711));
#16618=CARTESIAN_POINT('Ctrl Pts',(-0.0276126195379174,-0.136460326620484,
1.10334792136989));
#16619=CARTESIAN_POINT('Ctrl Pts',(0.0997182217817603,-0.0971604536002107,
1.11129008949267));
#16620=CARTESIAN_POINT('Ctrl Pts',(0.135696927507188,0.0311483765905046,
1.11923225761545));
#16621=CARTESIAN_POINT('Ctrl Pts',(0.0473633069609982,0.130922093830007,
1.12717442573822));
#16622=CARTESIAN_POINT('Ctrl Pts',(-0.0843599685788644,0.110757722983492,
1.13511659386101));
#16623=CARTESIAN_POINT('Ctrl Pts',(-0.138800846271631,-0.0108721006891078,
1.14305876198379));
#16624=CARTESIAN_POINT('Ctrl Pts',(-0.0660858892268601,-0.122541963197144,
1.15100093010657));
#16625=CARTESIAN_POINT('Ctrl Pts',(0.0671705316110708,-0.121950798202395,
1.15894309822935));
#16626=CARTESIAN_POINT('Ctrl Pts',(0.138891844802359,-0.00964017357273747,
1.16688526635212));
#16627=CARTESIAN_POINT('Ctrl Pts',(0.0833739592533277,0.111501840422208,
1.17482743447491));
#16628=CARTESIAN_POINT('Ctrl Pts',(-0.0485230383040216,0.130496713571114,
1.18276960259768));
#16629=CARTESIAN_POINT('Ctrl Pts',(-0.135967947813762,0.0299431906521225,
1.19071177072047));
#16630=CARTESIAN_POINT('Ctrl Pts',(-0.0988522486080867,-0.0980413710850678,
1.19865393884324));
#16631=CARTESIAN_POINT('Ctrl Pts',(0.0288222657999454,-0.136209964735594,
1.20659610696603));
#16632=CARTESIAN_POINT('Ctrl Pts',(0.130092623711363,-0.0495962373069701,
1.21453827508881));
#16633=CARTESIAN_POINT('Ctrl Pts',(0.112184773380136,0.082452738709893,
1.22248044321158));
#16634=CARTESIAN_POINT('Ctrl Pts',(-0.00849585454694533,0.138966535376798,
1.23042261133437));
#16635=CARTESIAN_POINT('Ctrl Pts',(-0.121393406896754,0.0681727090639588,
1.23836477945715));
#16636=CARTESIAN_POINT('Ctrl Pts',(-0.123082127310551,-0.0650743223999996,
1.24630694757992));
#16637=CARTESIAN_POINT('Ctrl Pts',(-0.0120149744006178,-0.138706589206355,
1.25424911570271));
#16638=CARTESIAN_POINT('Ctrl Pts',(0.110059129405696,-0.0852693704304675,
1.26219128382548));
#16639=CARTESIAN_POINT('Ctrl Pts',(0.13130776387206,0.0462833517151888,
1.27013345194827));
#16640=CARTESIAN_POINT('Ctrl Pts',(0.0322649968732001,0.135435768819968,
1.27807562007105));
#16641=CARTESIAN_POINT('Ctrl Pts',(-0.0963358219719167,0.100515107841202,
1.28601778819382));
#16642=CARTESIAN_POINT('Ctrl Pts',(-0.136683130933199,-0.0264877182308561,
1.29395995631661));
#16643=CARTESIAN_POINT('Ctrl Pts',(-0.0518146499729274,-0.129225073214149,
1.30190212443939));
#16644=CARTESIAN_POINT('Ctrl Pts',(0.0805213734929343,-0.11357898534207,
1.30984429256217));
#16645=CARTESIAN_POINT('Ctrl Pts',(0.1390915465469,0.0061171215252809,1.31778646068495));
#16646=CARTESIAN_POINT('Ctrl Pts',(0.0702395735793815,0.120209316621791,
1.32572862880773));
#16647=CARTESIAN_POINT('Ctrl Pts',(-0.0629590648350173,0.124177428154433,
1.33367079693051));
#16648=CARTESIAN_POINT('Ctrl Pts',(-0.138480731711197,0.0143862582011507,
1.34161296505328));
#16649=CARTESIAN_POINT('Ctrl Pts',(-0.0871398218994898,-0.108584202098263,
1.34955513317607));
#16650=CARTESIAN_POINT('Ctrl Pts',(0.0440301174146577,-0.132080378229483,
1.35749730129884));
#16651=CARTESIAN_POINT('Ctrl Pts',(0.13486394497766,-0.0345773583278084,
1.36543946942163));
#16652=CARTESIAN_POINT('Ctrl Pts',(0.102148545386143,0.0946020732301706,
1.3733816375444));
#16653=CARTESIAN_POINT('Ctrl Pts',(-0.0241454188302812,0.137116288461919,
1.38132380566719));
#16654=CARTESIAN_POINT('Ctrl Pts',(-0.128319693277533,0.0540178939468163,
1.38926597378996));
#16655=CARTESIAN_POINT('Ctrl Pts',(-0.114939956470138,-0.0785664351508689,
1.39720814191275));
#16656=CARTESIAN_POINT('Ctrl Pts',(0.00373660876362508,-0.139175849115243,
1.40515031003553));
#16657=CARTESIAN_POINT('Ctrl Pts',(0.118990018389619,-0.0722858665142316,
1.41309247815831));
#16658=CARTESIAN_POINT('Ctrl Pts',(0.125236419206141,0.0608253567263532,
1.42103464628109));
#16659=CARTESIAN_POINT('Ctrl Pts',(0.0167532566496359,0.13821437898841,
1.42897681440387));
#16660=CARTESIAN_POINT('Ctrl Pts',(-0.107077349343502,0.0889846891406984,
1.43691898252665));
#16661=CARTESIAN_POINT('Ctrl Pts',(-0.132814597987359,-0.0417638487589672,
1.44486115064943));
#16662=CARTESIAN_POINT('Ctrl Pts',(-0.0368790902657646,-0.134252921254984,
1.45280331877221));
#16663=CARTESIAN_POINT('Ctrl Pts',(0.0928396680879532,-0.103751556080299,
1.46074548689499));
#16664=CARTESIAN_POINT('Ctrl Pts',(0.137511141307062,0.0217950526079239,
1.46868765501776));
#16665=CARTESIAN_POINT('Ctrl Pts',(0.0562018483347667,0.127378648737854,
1.47662982314055));
#16666=CARTESIAN_POINT('Ctrl Pts',(-0.0765818961642769,0.116263681173923,
1.48457199126332));
#16667=CARTESIAN_POINT('Ctrl Pts',(-0.13923195096087,-0.00134816270381636,
1.49251415938611));
#16668=CARTESIAN_POINT('Ctrl Pts',(-0.0742871760264013,-0.117748889605885,
1.50045632750888));
#16669=CARTESIAN_POINT('Ctrl Pts',(0.0586284551779338,-0.126233948370975,
1.50839849563167));
#16670=CARTESIAN_POINT('Ctrl Pts',(0.137995068118234,-0.019163470063063,
1.51634066375444));
#16671=CARTESIAN_POINT('Ctrl Pts',(0.0906261803825392,0.105639137646141,
1.52428283187723));
#16672=CARTESIAN_POINT('Ctrl Pts',(0.00417072711528833,0.124051375507138,
1.52957761062575));
#16673=CARTESIAN_POINT('Ctrl Pts',(-0.0334019664627544,0.1129391839063,
1.53222500000001));
#16674=CARTESIAN_POINT('Ctrl Pts',(-0.0551480035117261,0.114734422509858,
-0.0109985226280628));
#16675=CARTESIAN_POINT('Ctrl Pts',(-0.093317938433455,0.0963877427684319,
-0.00835113325380276));
#16676=CARTESIAN_POINT('Ctrl Pts',(-0.149247407742026,0.0189255452031589,
-0.00305635450528277));
#16677=CARTESIAN_POINT('Ctrl Pts',(-0.0966876253720675,-0.115446371588928,
0.00488581361749726));
#16678=CARTESIAN_POINT('Ctrl Pts',(0.0445747075563756,-0.143685636564375,
0.0128279817402772));
#16679=CARTESIAN_POINT('Ctrl Pts',(0.144936900801175,-0.0404809362687151,
0.0207701498630572));
#16680=CARTESIAN_POINT('Ctrl Pts',(0.112556116319125,0.0999057960529736,
0.0287123179858373));
#16681=CARTESIAN_POINT('Ctrl Pts',(-0.0229555792165621,0.148717415239805,
0.0366544861086172));
#16682=CARTESIAN_POINT('Ctrl Pts',(-0.137428156769908,0.0613155244327884,
0.0445966542313972));
#16683=CARTESIAN_POINT('Ctrl Pts',(-0.126007400730642,-0.0822718633254329,
0.0525388223541772));
#16684=CARTESIAN_POINT('Ctrl Pts',(0.000851700720621877,-0.150482305134309,
0.0604809904769572));
#16685=CARTESIAN_POINT('Ctrl Pts',(0.126929176276611,-0.0808394286734405,
0.0684231585997372));
#16686=CARTESIAN_POINT('Ctrl Pts',(0.136727213562698,0.0628627408439891,
0.0763653267225173));
#16687=CARTESIAN_POINT('Ctrl Pts',(0.0212686937255662,0.148975090584026,
0.0843074948452972));
#16688=CARTESIAN_POINT('Ctrl Pts',(-0.113673932864549,0.0986115272026031,
0.0922496629680772));
#16689=CARTESIAN_POINT('Ctrl Pts',(-0.144479665027646,-0.0420906285100245,
0.100191831090857));
#16690=CARTESIAN_POINT('Ctrl Pts',(-0.0429271251068198,-0.144233284958223,
0.108133999213637));
#16691=CARTESIAN_POINT('Ctrl Pts',(0.0979510420095061,-0.114243518700172,
0.116076167336417));
#16692=CARTESIAN_POINT('Ctrl Pts',(0.149096007275942,0.0204050915936607,
0.124018335459197));
#16693=CARTESIAN_POINT('Ctrl Pts',(0.0636537044864716,0.136360518400275,
0.131960503581977));
#16694=CARTESIAN_POINT('Ctrl Pts',(-0.0801019266996435,0.127395713772213,
0.139902671704757));
#16695=CARTESIAN_POINT('Ctrl Pts',(-0.15047596611352,0.00172334100814176,
0.147844839827537));
#16696=CARTESIAN_POINT('Ctrl Pts',(-0.0829985603893774,-0.125527785761544,
0.155787007950317));
#16697=CARTESIAN_POINT('Ctrl Pts',(0.0605140527882773,-0.137782566606816,
0.163729176073097));
#16698=CARTESIAN_POINT('Ctrl Pts',(0.148589577098441,-0.0238143605552183,
0.171671344195877));
#16699=CARTESIAN_POINT('Ctrl Pts',(0.100541783424623,0.111970245809892,
0.179613512318657));
#16700=CARTESIAN_POINT('Ctrl Pts',(-0.0396126128240685,0.145178604134651,
0.187555680441437));
#16701=CARTESIAN_POINT('Ctrl Pts',(-0.143477786216001,0.0453884461694337,
0.195497848564217));
#16702=CARTESIAN_POINT('Ctrl Pts',(-0.115902567375552,-0.095982191346566,
0.203440016686997));
#16703=CARTESIAN_POINT('Ctrl Pts',(0.0178513102906219,-0.149423281002214,
0.211382184809777));
#16704=CARTESIAN_POINT('Ctrl Pts',(0.135251553802876,-0.0659772944027704,
0.219324352932557));
#16705=CARTESIAN_POINT('Ctrl Pts',(0.128747479107914,0.07791067196398,0.227266521055337));
#16706=CARTESIAN_POINT('Ctrl Pts',(0.00429748682099232,0.150424458749874,
0.235208689178117));
#16707=CARTESIAN_POINT('Ctrl Pts',(-0.124089444892588,0.0851339876261335,
0.243150857300897));
#16708=CARTESIAN_POINT('Ctrl Pts',(-0.138797696890977,-0.0581479623084488,
0.251093025423677));
#16709=CARTESIAN_POINT('Ctrl Pts',(-0.0263529993083425,-0.148160405002171,
0.259035193546457));
#16710=CARTESIAN_POINT('Ctrl Pts',(0.110233752987369,-0.102442695616748,
0.266977361669237));
#16711=CARTESIAN_POINT('Ctrl Pts',(0.145835062802846,0.0371230472913779,
0.274919529792017));
#16712=CARTESIAN_POINT('Ctrl Pts',(0.0478364728857143,0.142680265085169,
0.282861697914797));
#16713=CARTESIAN_POINT('Ctrl Pts',(-0.0939852406223356,0.117527701960322,
0.290803866037577));
#16714=CARTESIAN_POINT('Ctrl Pts',(-0.14970681824969,-0.01529231023972,
0.298746034160357));
#16715=CARTESIAN_POINT('Ctrl Pts',(-0.0682815703945392,-0.134102995221473,
0.306688202283137));
#16716=CARTESIAN_POINT('Ctrl Pts',(0.0756966107742644,-0.1300615596562,
0.314630370405917));
#16717=CARTESIAN_POINT('Ctrl Pts',(0.150328919865546,-0.00687037371415525,
0.322572538528697));
#16718=CARTESIAN_POINT('Ctrl Pts',(0.0872444944832666,0.122614780370367,
0.330514706651477));
#16719=CARTESIAN_POINT('Ctrl Pts',(-0.0557648508131485,0.139772198940638,
0.338456874774257));
#16720=CARTESIAN_POINT('Ctrl Pts',(-0.147687863823926,0.0288839239377102,
0.346399042897038));
#16721=CARTESIAN_POINT('Ctrl Pts',(-0.104313621021262,-0.10846499275041,
0.354341211019817));
#16722=CARTESIAN_POINT('Ctrl Pts',(0.0346226151823369,-0.146448833047075,
0.362283379142597));
#16723=CARTESIAN_POINT('Ctrl Pts',(0.141840978962514,-0.0502704970123603,
0.370225547265377));
#16724=CARTESIAN_POINT('Ctrl Pts',(0.119118434135606,0.0919607787700563,
0.378167715388157));
#16725=CARTESIAN_POINT('Ctrl Pts',(-0.0127288338612142,0.149946533709345,
0.386109883510937));
#16726=CARTESIAN_POINT('Ctrl Pts',(-0.132915182358376,0.070565859178174,
0.394052051633717));
#16727=CARTESIAN_POINT('Ctrl Pts',(-0.131337568919768,-0.0734603918663599,
0.401994219756497));
#16728=CARTESIAN_POINT('Ctrl Pts',(-0.00944124952954395,-0.150189377088511,
0.409936387879277));
#16729=CARTESIAN_POINT('Ctrl Pts',(0.121104224366159,-0.0893294633566384,
0.417878556002057));
#16730=CARTESIAN_POINT('Ctrl Pts',(0.140705787232781,0.0533654159743681,
0.425820724124838));
#16731=CARTESIAN_POINT('Ctrl Pts',(0.0314063937394313,0.147172091835368,
0.433762892247617));
#16732=CARTESIAN_POINT('Ctrl Pts',(-0.106664482920656,0.106154012011714,
0.441705060370398));
#16733=CARTESIAN_POINT('Ctrl Pts',(-0.147019735166745,-0.032112048430678,
0.449647228493177));
#16734=CARTESIAN_POINT('Ctrl Pts',(-0.052689806088835,-0.14096017351449,
0.457589396615958));
#16735=CARTESIAN_POINT('Ctrl Pts',(0.0899093983958942,-0.120674298270189,
0.465531564738737));
#16736=CARTESIAN_POINT('Ctrl Pts',(0.15014235720654,0.0101616315312987,
0.473473732861518));
#16737=CARTESIAN_POINT('Ctrl Pts',(0.0728294921055832,0.131688462906045,
0.481415900984297));
#16738=CARTESIAN_POINT('Ctrl Pts',(-0.071202669822089,0.132575133389036,
0.489358069107078));
#16739=CARTESIAN_POINT('Ctrl Pts',(-0.150005871264529,0.012009361726732,
0.497300237229857));
#16740=CARTESIAN_POINT('Ctrl Pts',(-0.0913882839399832,-0.119558219045865,
0.505242405352637));
#16741=CARTESIAN_POINT('Ctrl Pts',(0.0509503601487159,-0.141598188489932,
0.513184573475417));
#16742=CARTESIAN_POINT('Ctrl Pts',(0.146613240011817,-0.0339196703426114,
0.521126741598197));
#16743=CARTESIAN_POINT('Ctrl Pts',(0.107963329873666,0.104832750538675,
0.529068909720978));
#16744=CARTESIAN_POINT('Ctrl Pts',(-0.0295920819230583,0.147547602048875,
0.537011077843756));
#16745=CARTESIAN_POINT('Ctrl Pts',(-0.140038106568177,0.055093691941219,
0.544953245966537));
#16746=CARTESIAN_POINT('Ctrl Pts',(-0.122194838935542,-0.0878316999746162,
0.552895414089317));
#16747=CARTESIAN_POINT('Ctrl Pts',(0.00759145471482065,-0.150294231420327,
0.560837582212097));
#16748=CARTESIAN_POINT('Ctrl Pts',(0.130423195946632,-0.0750718065719766,
0.568779750334878));
#16749=CARTESIAN_POINT('Ctrl Pts',(0.133773890807325,0.0689241055160235,
0.576721918457657));
#16750=CARTESIAN_POINT('Ctrl Pts',(0.0145739585745413,0.149778456108953,
0.584664086580438));
#16751=CARTESIAN_POINT('Ctrl Pts',(-0.117977216952174,0.0934203535806499,
0.592606254703216));
#16752=CARTESIAN_POINT('Ctrl Pts',(-0.142449141490696,-0.0485203902651028,
0.600548422825998));
#16753=CARTESIAN_POINT('Ctrl Pts',(-0.036423018067407,-0.146011471938939,
0.608490590948776));
#16754=CARTESIAN_POINT('Ctrl Pts',(0.102970331784443,-0.109741044988262,
0.616432759071558));
#16755=CARTESIAN_POINT('Ctrl Pts',(0.148032279177632,0.0270634532975707,
0.624374927194337));
#16756=CARTESIAN_POINT('Ctrl Pts',(0.0574814509102497,0.139075048028633,
0.632317095317117));
#16757=CARTESIAN_POINT('Ctrl Pts',(-0.0857282916847416,0.123679611042927,
0.640259263439898));
#16758=CARTESIAN_POINT('Ctrl Pts',(-0.150402111894479,-0.00501905574730406,
0.648201431562677));
#16759=CARTESIAN_POINT('Ctrl Pts',(-0.0772921462128499,-0.129119751845818,
0.656143599685457));
#16760=CARTESIAN_POINT('Ctrl Pts',(0.0666253659236285,-0.134933490277457,
0.664085767808237));
#16761=CARTESIAN_POINT('Ctrl Pts',(0.14950719819016,-0.0171342893707992,
0.672027935931017));
#16762=CARTESIAN_POINT('Ctrl Pts',(0.0954250774564579,0.11636168087194,
0.679970104053797));
#16763=CARTESIAN_POINT('Ctrl Pts',(-0.0460762176180427,0.143258397146306,
0.687912272176577));
#16764=CARTESIAN_POINT('Ctrl Pts',(-0.145366963764729,0.0389157041403328,
0.695854440299358));
#16765=CARTESIAN_POINT('Ctrl Pts',(-0.111486636987321,-0.101077771820372,
0.703796608422136));
#16766=CARTESIAN_POINT('Ctrl Pts',(0.02452690272786,-0.148473624679578,
0.711738776544918));
#16767=CARTESIAN_POINT('Ctrl Pts',(0.138071279799868,-0.0598523840572839,
0.719680944667696));
#16768=CARTESIAN_POINT('Ctrl Pts',(0.125128179973684,0.0835997892305201,
0.727623112790477));
#16769=CARTESIAN_POINT('Ctrl Pts',(-0.00244518761474098,0.150465967050502,
0.735565280913257));
#16770=CARTESIAN_POINT('Ctrl Pts',(-0.127778512144395,0.0794898610961098,
0.743507449036036));
#16771=CARTESIAN_POINT('Ctrl Pts',(-0.136053592364468,-0.0643071239260258,
0.751449617158818));
#16772=CARTESIAN_POINT('Ctrl Pts',(-0.019689604662082,-0.149192176910068,
0.759391785281597));
#16773=CARTESIAN_POINT('Ctrl Pts',(0.114712083700712,-0.0974018687498071,
0.767333953404378));
#16774=CARTESIAN_POINT('Ctrl Pts',(0.144025718573537,0.0436185576594447,
0.775276121527157));
#16775=CARTESIAN_POINT('Ctrl Pts',(0.0413969989087525,0.14467990414796,
0.783218289649938));
#16776=CARTESIAN_POINT('Ctrl Pts',(-0.0991556246317344,0.113199594905656,
0.791160457772717));
#16777=CARTESIAN_POINT('Ctrl Pts',(-0.148871509365196,-0.021983172706469,
0.799102625895497));
#16778=CARTESIAN_POINT('Ctrl Pts',(-0.062205797368885,-0.137027095702329,
0.807044794018277));
#16779=CARTESIAN_POINT('Ctrl Pts',(0.081446815661698,-0.126540121706451,
0.814986962141057));
#16780=CARTESIAN_POINT('Ctrl Pts',(0.150485778196879,-0.000129396266831759,
0.822929130263837));
#16781=CARTESIAN_POINT('Ctrl Pts',(0.0816643079123276,0.126399869446589,
0.830871298386618));
#16782=CARTESIAN_POINT('Ctrl Pts',(-0.0619700581130299,0.137133869194964,
0.838813466509397));
#16783=CARTESIAN_POINT('Ctrl Pts',(-0.148833484480893,0.0222391564630926,
0.846755634632177));
#16784=CARTESIAN_POINT('Ctrl Pts',(-0.0993501488194509,-0.113028908304323,
0.854697802754957));
#16785=CARTESIAN_POINT('Ctrl Pts',(0.041148129789194,-0.144750881164039,
0.862639970877736));
#16786=CARTESIAN_POINT('Ctrl Pts',(0.143950494202948,-0.0438661760544617,
0.870582139000517));
#16787=CARTESIAN_POINT('Ctrl Pts',(0.114879417330645,0.0972044528644933,
0.878524307123298));
#16788=CARTESIAN_POINT('Ctrl Pts',(-0.0194330078274841,0.149225816766708,
0.886466475246077));
#16789=CARTESIAN_POINT('Ctrl Pts',(-0.135942801386891,0.0645410019599824,
0.894408643368857));
#16790=CARTESIAN_POINT('Ctrl Pts',(-0.127915022941288,-0.0792700011911429,
0.902350811491637));
#16791=CARTESIAN_POINT('Ctrl Pts',(-0.00270394227186439,-0.150461539534541,
0.910292979614417));
#16792=CARTESIAN_POINT('Ctrl Pts',(0.124984227305131,-0.0838148501630433,
0.918235147737197));
#16793=CARTESIAN_POINT('Ctrl Pts',(0.138174004553101,0.0596148525845174,
0.926177315859977));
#16794=CARTESIAN_POINT('Ctrl Pts',(0.0247821984756025,0.148431225898158,
0.934119483982757));
#16795=CARTESIAN_POINT('Ctrl Pts',(-0.11131264737753,0.101269347369872,
0.942061652105537));
#16796=CARTESIAN_POINT('Ctrl Pts',(-0.145433672650089,-0.0386656571445607,
0.950003820228317));
#16797=CARTESIAN_POINT('Ctrl Pts',(-0.0463225128062989,-0.143178947440692,
0.957945988351097));
#16798=CARTESIAN_POINT('Ctrl Pts',(0.0952248276606132,-0.116525612549003,
0.965888156473877));
#16799=CARTESIAN_POINT('Ctrl Pts',(0.149536443172165,0.0168771545685866,
0.973830324596656));
#16800=CARTESIAN_POINT('Ctrl Pts',(0.0668573142755158,0.134818714245386,
0.981772492719438));
#16801=CARTESIAN_POINT('Ctrl Pts',(-0.0770699830103684,0.129252481220654,
0.989714660842216));
#16802=CARTESIAN_POINT('Ctrl Pts',(-0.15039325815857,0.00527769678589187,
0.997656828964997));
#16803=CARTESIAN_POINT('Ctrl Pts',(-0.0859408583470751,-0.123532000103139,
1.00559899708778));
#16804=CARTESIAN_POINT('Ctrl Pts',(0.0572421967501742,-0.139173693973137,
1.01354116521056));
#16805=CARTESIAN_POINT('Ctrl Pts',(0.147985518909957,-0.0273179863069172,
1.02148333333334));
#16806=CARTESIAN_POINT('Ctrl Pts',(0.103158902618224,0.109563803299803,
1.02942550145612));
#16807=CARTESIAN_POINT('Ctrl Pts',(-0.0361718663885326,0.146073893166727,
1.0373676695789));
#16808=CARTESIAN_POINT('Ctrl Pts',(-0.142365489706367,0.0487652901517079,
1.04530983770168));
#16809=CARTESIAN_POINT('Ctrl Pts',(-0.118137698690712,-0.0932173284908804,
1.05325200582446));
#16810=CARTESIAN_POINT('Ctrl Pts',(0.0143163610725534,-0.149803297655807,
1.06119417394724));
#16811=CARTESIAN_POINT('Ctrl Pts',(0.133655163317704,-0.0691540562905145,
1.06913634207002));
#16812=CARTESIAN_POINT('Ctrl Pts',(0.130552105047211,0.0748474051030229,
1.0770785101928));
#16813=CARTESIAN_POINT('Ctrl Pts',(0.0078499064261323,0.150280954056111,
1.08502067831558));
#16814=CARTESIAN_POINT('Ctrl Pts',(-0.122043612932812,0.0880417101447944,
1.09296284643836));
#16815=CARTESIAN_POINT('Ctrl Pts',(-0.140132644828567,-0.0548527851276936,
1.10090501456114));
#16816=CARTESIAN_POINT('Ctrl Pts',(-0.0298457776877653,-0.147496493982489,
1.10884718268392));
#16817=CARTESIAN_POINT('Ctrl Pts',(0.107782887988268,-0.10501826145877,
1.1167893508067));
#16818=CARTESIAN_POINT('Ctrl Pts',(0.146671355310253,0.033667487497105,
1.12473151892948));
#16819=CARTESIAN_POINT('Ctrl Pts',(0.0511937930472066,0.141510359113225,
1.13267368705226));
#16820=CARTESIAN_POINT('Ctrl Pts',(-0.0911825429852659,0.119715203870077,
1.14061585517504));
#16821=CARTESIAN_POINT('Ctrl Pts',(-0.150026302104679,-0.0117513769282424,
1.14855802329782));
#16822=CARTESIAN_POINT('Ctrl Pts',(-0.0714305557085884,-0.132452489195471,
1.1565001914206));
#16823=CARTESIAN_POINT('Ctrl Pts',(0.0726029180563751,-0.131813513998426,
1.16444235954338));
#16824=CARTESIAN_POINT('Ctrl Pts',(0.150124660100533,-0.010419818262018,
1.17238452766616));
#16825=CARTESIAN_POINT('Ctrl Pts',(0.0901167906002831,0.120519501471002,
1.18032669578894));
#16826=CARTESIAN_POINT('Ctrl Pts',(-0.0524473171394798,0.141050576417769,
1.18826886391172));
#16827=CARTESIAN_POINT('Ctrl Pts',(-0.146964294261872,0.0323648326895764,
1.1962110320345));
#16828=CARTESIAN_POINT('Ctrl Pts',(-0.106846879624786,-0.105970422747861,
1.20415320015727));
#16829=CARTESIAN_POINT('Ctrl Pts',(0.0311532535456026,-0.14722588419309,
1.21209536828006));
#16830=CARTESIAN_POINT('Ctrl Pts',(0.140613805972886,-0.0536073106276968,
1.22003753640283));
#16831=CARTESIAN_POINT('Ctrl Pts',(0.121257666323848,0.0891210667609394,
1.22797970452562));
#16832=CARTESIAN_POINT('Ctrl Pts',(-0.00918295295119051,0.150205391241489,
1.2359218726484));
#16833=CARTESIAN_POINT('Ctrl Pts',(-0.131211043922368,0.0736861461587066,
1.24386404077118));
#16834=CARTESIAN_POINT('Ctrl Pts',(-0.133036338837895,-0.0703371788708997,
1.25180620889396));
#16835=CARTESIAN_POINT('Ctrl Pts',(-0.0129866800356469,-0.149924422041766,
1.25974837701674));
#16836=CARTESIAN_POINT('Ctrl Pts',(0.118960111851797,-0.0921654923014072,
1.26769054513952));
#16837=CARTESIAN_POINT('Ctrl Pts',(0.141927220045961,0.050026496908035,
1.2756327132623));
#16838=CARTESIAN_POINT('Ctrl Pts',(0.0348744139414821,0.146389075532006,
1.28357488138508));
#16839=CARTESIAN_POINT('Ctrl Pts',(-0.104126938119509,0.108644221848311,
1.29151704950786));
#16840=CARTESIAN_POINT('Ctrl Pts',(-0.147737317493493,-0.0286299004949125,
1.29945921763064));
#16841=CARTESIAN_POINT('Ctrl Pts',(-0.0560051364173496,-0.139676092720537,
1.30740138575342));
#16842=CARTESIAN_POINT('Ctrl Pts',(0.0870335032532438,-0.122764634549313,
1.3153435538762));
#16843=CARTESIAN_POINT('Ctrl Pts',(0.150340512633584,0.00661184096937889,
1.32328572199898));
#16844=CARTESIAN_POINT('Ctrl Pts',(0.0759201674095095,0.129931190880528,
1.33122789012176));
#16845=CARTESIAN_POINT('Ctrl Pts',(-0.0680508508044829,0.134220221643466,
1.33917005824454));
#16846=CARTESIAN_POINT('Ctrl Pts',(-0.149680298423566,0.0155497403439283,
1.34711222636732));
#16847=CARTESIAN_POINT('Ctrl Pts',(-0.0941872156892785,-0.117365900463673,
1.3550543944901));
#16848=CARTESIAN_POINT('Ctrl Pts',(0.0475910332998192,-0.142762319241037,
1.36299656261288));
#16849=CARTESIAN_POINT('Ctrl Pts',(0.145771005694385,-0.0373737865856905,
1.37093873073566));
#16850=CARTESIAN_POINT('Ctrl Pts',(0.110409762917901,0.10225297323032,1.37888089885844));
#16851=CARTESIAN_POINT('Ctrl Pts',(-0.0260981686868614,0.148205506441964,
1.38682306698121));
#16852=CARTESIAN_POINT('Ctrl Pts',(-0.138697490589939,0.0583865667538053,
1.394765235104));
#16853=CARTESIAN_POINT('Ctrl Pts',(-0.124235673603468,-0.0849204601545819,
1.40270740322677));
#16854=CARTESIAN_POINT('Ctrl Pts',(0.0040388053119065,-0.150431633134115,
1.41064957134956));
#16855=CARTESIAN_POINT('Ctrl Pts',(0.12861328245382,-0.0781319533624403,
1.41859173947234));
#16856=CARTESIAN_POINT('Ctrl Pts',(0.1353648581188,0.0657445800149866,1.42653390759512));
#16857=CARTESIAN_POINT('Ctrl Pts',(0.0181081687242482,0.149392404544468,
1.43447607571789));
#16858=CARTESIAN_POINT('Ctrl Pts',(-0.115737181672069,0.0961812857364522,
1.44241824384068));
#16859=CARTESIAN_POINT('Ctrl Pts',(-0.143555918690644,-0.0451414811888502,
1.45036041196346));
#16860=CARTESIAN_POINT('Ctrl Pts',(-0.0398616700558823,-0.145110565703753,
1.45830258008624));
#16861=CARTESIAN_POINT('Ctrl Pts',(0.100348034367198,-0.112142416378873,
1.46624474820902));
#16862=CARTESIAN_POINT('Ctrl Pts',(0.14863229283285,0.0235577176564554,
1.4741869163318));
#16863=CARTESIAN_POINT('Ctrl Pts',(0.0607471474677608,0.137680339497592,
1.48212908445458));
#16864=CARTESIAN_POINT('Ctrl Pts',(-0.0827754224726193,0.125666453945577,
1.49007125257736));
#16865=CARTESIAN_POINT('Ctrl Pts',(-0.150492272191201,-0.00145719475437189,
1.49801342070014));
#16866=CARTESIAN_POINT('Ctrl Pts',(-0.0802951178786721,-0.12727177793954,
1.50595558882292));
#16867=CARTESIAN_POINT('Ctrl Pts',(0.0633700050447994,-0.136443062004882,
1.5138977569457));
#16868=CARTESIAN_POINT('Ctrl Pts',(0.149155357006591,-0.0207133070603065,
1.52183992506848));
#16869=CARTESIAN_POINT('Ctrl Pts',(0.0979555318420461,0.114182655252422,
1.52978209319126));
#16870=CARTESIAN_POINT('Ctrl Pts',(0.00450803278943675,0.134083974545181,
1.53507687193978));
#16871=CARTESIAN_POINT('Ctrl Pts',(-0.0361033354337414,0.122073089461022,
1.53772426131404));
#16872=CARTESIAN_POINT('Ctrl Pts',(-0.0592743564846203,0.123319225136773,
-0.00549926131403157));
#16873=CARTESIAN_POINT('Ctrl Pts',(-0.100300290071938,0.10359978715075,
-0.00285187193977157));
#16874=CARTESIAN_POINT('Ctrl Pts',(-0.160414584165772,0.0203416160441626,
0.00244290680874841));
#16875=CARTESIAN_POINT('Ctrl Pts',(-0.103922107946056,-0.124084444561314,
0.0103850749315284));
#16876=CARTESIAN_POINT('Ctrl Pts',(0.0479099321398382,-0.154436663180837,
0.0183272430543084));
#16877=CARTESIAN_POINT('Ctrl Pts',(0.155781551077148,-0.0435098515708298,
0.0262694111770884));
#16878=CARTESIAN_POINT('Ctrl Pts',(0.120977930992648,0.107381072623318,
0.0342115792998684));
#16879=CARTESIAN_POINT('Ctrl Pts',(-0.0246731903087699,0.159844935900913,
0.0421537474226484));
#16880=CARTESIAN_POINT('Ctrl Pts',(-0.147710978397823,0.0659033513787588,
0.0500959155454284));
#16881=CARTESIAN_POINT('Ctrl Pts',(-0.135435684249567,-0.0884277117007276,
0.0580380836682085));
#16882=CARTESIAN_POINT('Ctrl Pts',(0.000915427738408385,-0.16174188059703,
0.0659802517909884));
#16883=CARTESIAN_POINT('Ctrl Pts',(0.13642643003965,-0.0868880976295618,
0.0739224199137684));
#16884=CARTESIAN_POINT('Ctrl Pts',(0.146957588340267,0.0675663355536457,
0.0818645880365484));
#16885=CARTESIAN_POINT('Ctrl Pts',(0.0228600865593111,0.160121891352391,
0.0898067561593285));
#16886=CARTESIAN_POINT('Ctrl Pts',(-0.122179386207322,0.105989962368389,
0.0977489242821083));
#16887=CARTESIAN_POINT('Ctrl Pts',(-0.155290103436038,-0.0452399862206161,
0.105691092404888));
#16888=CARTESIAN_POINT('Ctrl Pts',(-0.0461390722131997,-0.155025288408554,
0.113633260527668));
#16889=CARTESIAN_POINT('Ctrl Pts',(0.105280057525145,-0.122791590307548,
0.121575428650448));
#16890=CARTESIAN_POINT('Ctrl Pts',(0.160251855424436,0.0219318669073289,
0.129517596773229));
#16891=CARTESIAN_POINT('Ctrl Pts',(0.0684164816681947,0.146563455853242,
0.137459764896008));
#16892=CARTESIAN_POINT('Ctrl Pts',(-0.086095413359615,0.136927875387926,
0.145401933018789));
#16893=CARTESIAN_POINT('Ctrl Pts',(-0.16173506727009,0.00185228698694943,
0.153344101141568));
#16894=CARTESIAN_POINT('Ctrl Pts',(-0.0892087826023274,-0.134920182928699,
0.161286269264348));
#16895=CARTESIAN_POINT('Ctrl Pts',(0.0650419110192955,-0.148091906331324,
0.169228437387128));
#16896=CARTESIAN_POINT('Ctrl Pts',(0.159707532494063,-0.025596228460074,
0.177170605509908));
#16897=CARTESIAN_POINT('Ctrl Pts',(0.108064646638443,0.120348223746572,
0.185112773632688));
#16898=CARTESIAN_POINT('Ctrl Pts',(-0.0425765573421325,0.156041339440091,
0.193054941755468));
#16899=CARTESIAN_POINT('Ctrl Pts',(-0.154213260793436,0.0487845573223287,
0.200997109878248));
#16900=CARTESIAN_POINT('Ctrl Pts',(-0.124574774400312,-0.103163891052585,
0.208939278001028));
#16901=CARTESIAN_POINT('Ctrl Pts',(0.0191870033818907,-0.160603616835255,
0.216881446123808));
#16902=CARTESIAN_POINT('Ctrl Pts',(0.145371514918136,-0.0709139301387177,
0.224823614246588));
#16903=CARTESIAN_POINT('Ctrl Pts',(0.138380784202201,0.0837402018183176,
0.232765782369368));
#16904=CARTESIAN_POINT('Ctrl Pts',(0.00461903876105218,0.161679705957985,
0.240707950492149));
#16905=CARTESIAN_POINT('Ctrl Pts',(-0.133374220718213,0.0915039894496894,
0.248650118614928));
#16906=CARTESIAN_POINT('Ctrl Pts',(-0.149182991964712,-0.0624987819548612,
0.256592286737709));
#16907=CARTESIAN_POINT('Ctrl Pts',(-0.0283248164207669,-0.159246248345813,
0.264534454860488));
#16908=CARTESIAN_POINT('Ctrl Pts',(0.118481800883715,-0.110107791262854,
0.272476622983269));
#16909=CARTESIAN_POINT('Ctrl Pts',(0.156746916480749,0.0399007144198201,
0.280418791106048));
#16910=CARTESIAN_POINT('Ctrl Pts',(0.0514157533588968,0.153356066537929,
0.288360959228829));
#16911=CARTESIAN_POINT('Ctrl Pts',(-0.101017521980764,0.126321506839912,
0.296303127351608));
#16912=CARTESIAN_POINT('Ctrl Pts',(-0.160908369261695,-0.0164365306249019,
0.304245295474388));
#16913=CARTESIAN_POINT('Ctrl Pts',(-0.0733906195540655,-0.144137017448375,
0.312187463597168));
#16914=CARTESIAN_POINT('Ctrl Pts',(0.0813604773699057,-0.13979318853071,
0.320129631719948));
#16915=CARTESIAN_POINT('Ctrl Pts',(0.161577018543625,-0.00738443741900211,
0.328071799842729));
#16916=CARTESIAN_POINT('Ctrl Pts',(0.0937724112935796,0.131789217000595,
0.336013967965508));
#16917=CARTESIAN_POINT('Ctrl Pts',(-0.0599373583072218,0.150230409426965,
0.343956136088289));
#16918=CARTESIAN_POINT('Ctrl Pts',(-0.158738350099833,0.0310451130618767,
0.351898304211068));
#16919=CARTESIAN_POINT('Ctrl Pts',(-0.112118705390683,-0.116580696253536,
0.359840472333849));
#16920=CARTESIAN_POINT('Ctrl Pts',(0.0372131918485748,-0.15740661101073,
0.367782640456628));
#16921=CARTESIAN_POINT('Ctrl Pts',(0.152453982298084,-0.0540318990865351,
0.375724808579408));
#16922=CARTESIAN_POINT('Ctrl Pts',(0.128031262769868,0.0988415833088236,
0.383666976702188));
#16923=CARTESIAN_POINT('Ctrl Pts',(-0.0136812466069205,0.161166021011634,
0.391609144824968));
#16924=CARTESIAN_POINT('Ctrl Pts',(-0.142860328563903,0.0758458262533652,
0.399551312947749));
#16925=CARTESIAN_POINT('Ctrl Pts',(-0.141164672957165,-0.0789569372907697,
0.407493481070528));
#16926=CARTESIAN_POINT('Ctrl Pts',(-0.0101476745237983,-0.161427034722196,
0.415435649193308));
#16927=CARTESIAN_POINT('Ctrl Pts',(0.130165636283581,-0.0960133843187101,
0.423377817316089));
#16928=CARTESIAN_POINT('Ctrl Pts',(0.151233851831306,0.0573583899504574,
0.431319985438868));
#16929=CARTESIAN_POINT('Ctrl Pts',(0.0337563222576384,0.158183986373718,
0.439262153561649));
#16930=CARTESIAN_POINT('Ctrl Pts',(-0.114645466422773,0.114096800420287,
0.447204321684428));
#16931=CARTESIAN_POINT('Ctrl Pts',(-0.158020229883659,-0.0345147763277912,
0.455146489807208));
#16932=CARTESIAN_POINT('Ctrl Pts',(-0.0566322287360923,-0.151507272121918,
0.463088657929988));
#16933=CARTESIAN_POINT('Ctrl Pts',(0.0966367119836487,-0.129703541718919,
0.471030826052768));
#16934=CARTESIAN_POINT('Ctrl Pts',(0.161376496659739,0.0109219578497271,
0.478972994175549));
#16935=CARTESIAN_POINT('Ctrl Pts',(0.0782788315581001,0.141541821972661,
0.486915162298328));
#16936=CARTESIAN_POINT('Ctrl Pts',(-0.0765302851406724,0.142494836024782,
0.494857330421108));
#16937=CARTESIAN_POINT('Ctrl Pts',(-0.161229798395673,0.0129079412274925,
0.502799498543889));
#16938=CARTESIAN_POINT('Ctrl Pts',(-0.0982262525537151,-0.128503953817366,
0.510741666666668));
#16939=CARTESIAN_POINT('Ctrl Pts',(0.0547626317937811,-0.152193025452748,
0.518683834789449));
#16940=CARTESIAN_POINT('Ctrl Pts',(0.157583319439253,-0.0364576503898468,
0.526626002912228));
#16941=CARTESIAN_POINT('Ctrl Pts',(0.116041497328862,0.112676677866884,
0.534568171035008));
#16942=CARTESIAN_POINT('Ctrl Pts',(-0.0318062577307366,0.158587593482618,
0.542510339157789));
#16943=CARTESIAN_POINT('Ctrl Pts',(-0.150516213127973,0.0592159811457737,
0.550452507280567));
#16944=CARTESIAN_POINT('Ctrl Pts',(-0.131337854181896,-0.0944035534094825,
0.558394675403349));
#16945=CARTESIAN_POINT('Ctrl Pts',(0.00815947204521347,-0.161539734596121,
0.566336843526128));
#16946=CARTESIAN_POINT('Ctrl Pts',(0.140181883624494,-0.080688923285235,
0.574279011648909));
#16947=CARTESIAN_POINT('Ctrl Pts',(0.143783288371658,0.0740812312429708,
0.582221179771688));
#16948=CARTESIAN_POINT('Ctrl Pts',(0.0156644295519346,0.160985367298567,
0.590163347894469));
#16949=CARTESIAN_POINT('Ctrl Pts',(-0.126804656005353,0.100410368253513,
0.598105516017247));
#16950=CARTESIAN_POINT('Ctrl Pts',(-0.153107649524464,-0.0521508436608248,
0.606047684140029));
#16951=CARTESIAN_POINT('Ctrl Pts',(-0.0391483067326994,-0.156936525122116,
0.613989852262808));
#16952=CARTESIAN_POINT('Ctrl Pts',(0.110674906884577,-0.117952226869747,
0.621932020385589));
#16953=CARTESIAN_POINT('Ctrl Pts',(0.159108535730396,0.0290884288879846,
0.629874188508368));
#16954=CARTESIAN_POINT('Ctrl Pts',(0.061782400006242,0.14948109541648,0.637816356631148));
#16955=CARTESIAN_POINT('Ctrl Pts',(-0.0921427612707386,0.132933721767072,
0.645758524753929));
#16956=CARTESIAN_POINT('Ctrl Pts',(-0.161655687038194,-0.0053945978210935,
0.653700692876707));
#16957=CARTESIAN_POINT('Ctrl Pts',(-0.0830753959589387,-0.138780911597048,
0.661642860999489));
#16958=CARTESIAN_POINT('Ctrl Pts',(0.0716104924784035,-0.145029652845349,
0.669585029122267));
#16959=CARTESIAN_POINT('Ctrl Pts',(0.160693812980115,-0.0184163326249747,
0.677527197245049));
#16960=CARTESIAN_POINT('Ctrl Pts',(0.102565092089392,0.125068240261613,
0.685469365367828));
#16961=CARTESIAN_POINT('Ctrl Pts',(-0.0495237900674707,0.153977456320057,
0.693411533490608));
#16962=CARTESIAN_POINT('Ctrl Pts',(-0.156243792750268,0.0418275036842162,
0.701353701613389));
#16963=CARTESIAN_POINT('Ctrl Pts',(-0.119828429739121,-0.108640739429086,
0.709295869736167));
#16964=CARTESIAN_POINT('Ctrl Pts',(0.0263620853553792,-0.159582904138124,
0.717238037858949));
#16965=CARTESIAN_POINT('Ctrl Pts',(0.148402221984423,-0.0643307340819919,
0.725180205981728));
#16966=CARTESIAN_POINT('Ctrl Pts',(0.134490677336207,0.0898549973406614,
0.733122374104509));
#16967=CARTESIAN_POINT('Ctrl Pts',(-0.00262814450422035,0.161724320044658,
0.741064542227287));
#16968=CARTESIAN_POINT('Ctrl Pts',(-0.137339315979238,0.0854375510170853,
0.749006710350069));
#16969=CARTESIAN_POINT('Ctrl Pts',(-0.146233564613262,-0.0691187920752458,
0.756948878472847));
#16970=CARTESIAN_POINT('Ctrl Pts',(-0.0211628449166461,-0.160355220783347,
0.764891046595629));
#16971=CARTESIAN_POINT('Ctrl Pts',(0.12329521486528,-0.104689793336152,
0.772833214718408));
#16972=CARTESIAN_POINT('Ctrl Pts',(0.154802191231926,0.0468822399980663,
0.780775382841188));
#16973=CARTESIAN_POINT('Ctrl Pts',(0.0444944569967772,0.155505325098544,
0.788717550963968));
#16974=CARTESIAN_POINT('Ctrl Pts',(-0.106574770936664,0.121669556739719,
0.796659719086747));
#16975=CARTESIAN_POINT('Ctrl Pts',(-0.160010559849905,-0.0236280251811701,
0.804601887209529));
#16976=CARTESIAN_POINT('Ctrl Pts',(-0.0668602374312443,-0.147279908636853,
0.812544055332307));
#16977=CARTESIAN_POINT('Ctrl Pts',(0.0875409312876049,-0.13600826514128,
0.820486223455089));
#16978=CARTESIAN_POINT('Ctrl Pts',(0.161745613525436,-0.000139078116330951,
0.828428391577867));
#16979=CARTESIAN_POINT('Ctrl Pts',(0.0877746970157421,0.135857518751215,
0.836370559700649));
#16980=CARTESIAN_POINT('Ctrl Pts',(-0.0666068593976089,0.147394671269449,
0.844312727823428));
#16981=CARTESIAN_POINT('Ctrl Pts',(-0.159969689820096,0.0239031624749592,
0.852254895946208));
#16982=CARTESIAN_POINT('Ctrl Pts',(-0.106783850056725,-0.121486098811777,
0.860197064068988));
#16983=CARTESIAN_POINT('Ctrl Pts',(0.0442269666803361,-0.155581612845794,
0.868139232191768));
#16984=CARTESIAN_POINT('Ctrl Pts',(0.154721338329289,-0.0471483860066884,
0.876081400314548));
#16985=CARTESIAN_POINT('Ctrl Pts',(0.123475068941597,0.104477606152275,
0.884023568437328));
#16986=CARTESIAN_POINT('Ctrl Pts',(-0.0208870486723946,0.160391377683462,
0.891965736560109));
#16987=CARTESIAN_POINT('Ctrl Pts',(-0.146114483894434,0.0693701696243073,
0.899907904682887));
#16988=CARTESIAN_POINT('Ctrl Pts',(-0.137486040957907,-0.0852012404790134,
0.907850072805669));
#16989=CARTESIAN_POINT('Ctrl Pts',(-0.00290626002629624,-0.161719561247554,
0.915792240928448));
#16990=CARTESIAN_POINT('Ctrl Pts',(0.134335953660838,-0.0900861498315643,
0.923734409051229));
#16991=CARTESIAN_POINT('Ctrl Pts',(0.148512632937768,0.0640754297319473,
0.931676577174007));
#16992=CARTESIAN_POINT('Ctrl Pts',(0.0266364831612253,0.159537332941991,
0.939618745296788));
#16993=CARTESIAN_POINT('Ctrl Pts',(-0.119641421660886,0.10884664928423,
0.947560913419568));
#16994=CARTESIAN_POINT('Ctrl Pts',(-0.156315493011378,-0.0415587473590326,
0.955503081542348));
#16995=CARTESIAN_POINT('Ctrl Pts',(-0.0497885138626987,-0.153892061929087,
0.963445249665127));
#16996=CARTESIAN_POINT('Ctrl Pts',(0.102349858952582,-0.125244437839883,
0.971387417787908));
#16997=CARTESIAN_POINT('Ctrl Pts',(0.160725246166783,0.018139958160622,
0.979329585910688));
#16998=CARTESIAN_POINT('Ctrl Pts',(0.0718597959603077,0.14490628889729,
0.987271754033468));
#16999=CARTESIAN_POINT('Ctrl Pts',(-0.0828366097831417,0.138923572215364,
0.995213922156248));
#17000=CARTESIAN_POINT('Ctrl Pts',(-0.161646170836971,0.00567259122332548,
1.00315609027903));
#17001=CARTESIAN_POINT('Ctrl Pts',(-0.0923712328620446,-0.132775066096718,
1.01109825840181));
#17002=CARTESIAN_POINT('Ctrl Pts',(0.0615252440718216,-0.149587122371362,
1.01904042652459));
#17003=CARTESIAN_POINT('Ctrl Pts',(0.159058276707423,-0.0293620068848675,
1.02698259464737));
#17004=CARTESIAN_POINT('Ctrl Pts',(0.1108775872014,0.117761723381742,1.03492476277015));
#17005=CARTESIAN_POINT('Ctrl Pts',(-0.0388783630684312,0.157003616909169,
1.04286693089293));
#17006=CARTESIAN_POINT('Ctrl Pts',(-0.153017738641585,0.0524140677533946,
1.05080909901571));
#17007=CARTESIAN_POINT('Ctrl Pts',(-0.126977145509477,-0.10019215216626,
1.05875126713849));
#17008=CARTESIAN_POINT('Ctrl Pts',(0.0153875577671049,-0.161012067570745,
1.06669343526127));
#17009=CARTESIAN_POINT('Ctrl Pts',(0.143655677305146,-0.0743283876822416,
1.07463560338405));
#17010=CARTESIAN_POINT('Ctrl Pts',(0.140320438123209,0.080447731368589,
1.08257777150683));
#17011=CARTESIAN_POINT('Ctrl Pts',(0.00843726195408678,0.161525463776335,
1.09051993962961));
#17012=CARTESIAN_POINT('Ctrl Pts',(-0.131175312957834,0.094629277223576,
1.09846210775239));
#17013=CARTESIAN_POINT('Ctrl Pts',(-0.150617825048456,-0.0589570489009974,
1.10640427587517));
#17014=CARTESIAN_POINT('Ctrl Pts',(-0.0320789358376135,-0.158532661344495,
1.11434644399795));
#17015=CARTESIAN_POINT('Ctrl Pts',(0.115847554194776,-0.112876069317329,
1.12228861212073));
#17016=CARTESIAN_POINT('Ctrl Pts',(0.157645783113317,0.0361865984037055,
1.13023078024351));
#17017=CARTESIAN_POINT('Ctrl Pts',(0.0550242791334153,0.152098624396442,
1.13817294836629));
#17018=CARTESIAN_POINT('Ctrl Pts',(-0.0980051173916675,0.128672684756662,
1.14611511648907));
#17019=CARTESIAN_POINT('Ctrl Pts',(-0.161251757937727,-0.0126306531673768,
1.15405728461185));
#17020=CARTESIAN_POINT('Ctrl Pts',(-0.0767752221903169,-0.142363015193798,
1.16199945273463));
#17021=CARTESIAN_POINT('Ctrl Pts',(0.0780353045016797,-0.141676229794458,
1.16994162085741));
#17022=CARTESIAN_POINT('Ctrl Pts',(0.161357475398708,-0.0111994629512984,
1.17788378898019));
#17023=CARTESIAN_POINT('Ctrl Pts',(0.0968596219472387,0.129537162519796,
1.18582595710297));
#17024=CARTESIAN_POINT('Ctrl Pts',(-0.0563715959749383,0.151604439264423,
1.19376812522575));
#17025=CARTESIAN_POINT('Ctrl Pts',(-0.157960640709981,0.0347864747270306,
1.20171029334853));
#17026=CARTESIAN_POINT('Ctrl Pts',(-0.114841510641486,-0.113899474410655,
1.20965246147131));
#17027=CARTESIAN_POINT('Ctrl Pts',(0.03348424129126,-0.158241803650584,
1.21759462959409));
#17028=CARTESIAN_POINT('Ctrl Pts',(0.151134988234409,-0.0576183839484237,
1.22553679771687));
#17029=CARTESIAN_POINT('Ctrl Pts',(0.130330559267559,0.0957893948119858,
1.23347896583965));
#17030=CARTESIAN_POINT('Ctrl Pts',(-0.0098700513554357,0.16144424710618,
1.24142113396243));
#17031=CARTESIAN_POINT('Ctrl Pts',(-0.141028680947982,0.0791995832534545,
1.24936330208521));
#17032=CARTESIAN_POINT('Ctrl Pts',(-0.142990550365238,-0.0756000353418,
1.25730547020799));
#17033=CARTESIAN_POINT('Ctrl Pts',(-0.013958385670676,-0.161142254877177,
1.26524763833077));
#17034=CARTESIAN_POINT('Ctrl Pts',(0.127861094297897,-0.0990616141723472,
1.27318980645355));
#17035=CARTESIAN_POINT('Ctrl Pts',(0.152546676219863,0.0537696421008814,
1.28113197457633));
#17036=CARTESIAN_POINT('Ctrl Pts',(0.0374838310097642,0.157342382244044,
1.28907414269911));
#17037=CARTESIAN_POINT('Ctrl Pts',(-0.111918054267102,0.116773335855419,
1.29701631082189));
#17038=CARTESIAN_POINT('Ctrl Pts',(-0.158791504053787,-0.0307720827589687,
1.30495847894467));
#17039=CARTESIAN_POINT('Ctrl Pts',(-0.060195622861772,-0.150127112226926,
1.31290064706745));
#17040=CARTESIAN_POINT('Ctrl Pts',(0.0935456330135535,-0.131950283756556,
1.32084281519023));
#17041=CARTESIAN_POINT('Ctrl Pts',(0.161589478720268,0.00710656041347678,
1.32878498331301));
#17042=CARTESIAN_POINT('Ctrl Pts',(0.0816007612396376,0.139653065139265,
1.33672715143579));
#17043=CARTESIAN_POINT('Ctrl Pts',(-0.0731426367739486,0.144263015132499,
1.34466931955857));
#17044=CARTESIAN_POINT('Ctrl Pts',(-0.160879865135934,0.0167132224867059,
1.35261148768135));
#17045=CARTESIAN_POINT('Ctrl Pts',(-0.101234609479067,-0.126147598829082,
1.36055365580413));
#17046=CARTESIAN_POINT('Ctrl Pts',(0.051151949184981,-0.153444260252591,
1.36849582392691));
#17047=CARTESIAN_POINT('Ctrl Pts',(0.15667806641111,-0.0401702148435725,
1.37643799204969));
#17048=CARTESIAN_POINT('Ctrl Pts',(0.118670980449659,0.10990387323047,1.38438016017247));
#17049=CARTESIAN_POINT('Ctrl Pts',(-0.0280509185434417,0.159294724422008,
1.39232232829525));
#17050=CARTESIAN_POINT('Ctrl Pts',(-0.149075287902345,0.0627552395607943,
1.40026449641803));
#17051=CARTESIAN_POINT('Ctrl Pts',(-0.133531390736797,-0.0912744851582948,
1.40820666454081));
#17052=CARTESIAN_POINT('Ctrl Pts',(0.00434100186018791,-0.161687417152987,
1.41614883266359));
#17053=CARTESIAN_POINT('Ctrl Pts',(0.138236546518021,-0.0839780402106489,
1.42409100078637));
#17054=CARTESIAN_POINT('Ctrl Pts',(0.145493297031458,0.07066380330362,1.43203316890915));
#17055=CARTESIAN_POINT('Ctrl Pts',(0.0194630807988606,0.160570430100525,
1.43997533703193));
#17056=CARTESIAN_POINT('Ctrl Pts',(-0.124397014000637,0.103377882332206,
1.44791750515471));
#17057=CARTESIAN_POINT('Ctrl Pts',(-0.15429723939393,-0.0485191136187331,
1.45585967327749));
#17058=CARTESIAN_POINT('Ctrl Pts',(-0.042844249846,-0.155968210152522,1.46380184140027));
#17059=CARTESIAN_POINT('Ctrl Pts',(0.107856400646442,-0.120533276677448,
1.47174400952305));
#17060=CARTESIAN_POINT('Ctrl Pts',(0.159753444358638,0.0253203827049868,
1.47968617764583));
#17061=CARTESIAN_POINT('Ctrl Pts',(0.0652924466007548,0.147982030257331,
1.48762834576861));
#17062=CARTESIAN_POINT('Ctrl Pts',(-0.0889689487809616,0.13506922671723,
1.49557051389139));
#17063=CARTESIAN_POINT('Ctrl Pts',(-0.161752593421533,-0.00156622680492735,
1.50351268201417));
#17064=CARTESIAN_POINT('Ctrl Pts',(-0.086303059730943,-0.136794666273195,
1.51145485013695));
#17065=CARTESIAN_POINT('Ctrl Pts',(0.0681115549116652,-0.14665217563879,
1.51939701825973));
#17066=CARTESIAN_POINT('Ctrl Pts',(0.160315645894948,-0.02226314405755,
1.52733918638251));
#17067=CARTESIAN_POINT('Ctrl Pts',(0.105284883301553,0.122726172858702,
1.53528135450529));
#17068=CARTESIAN_POINT('Ctrl Pts',(0.00484533846358528,0.144116573583224,
1.54057613325381));
#17069=CARTESIAN_POINT('Ctrl Pts',(-0.0388047044047284,0.131206995015745,
1.54322352262807));
#17070=CARTESIAN_POINT('Ctrl Pts',(-0.0634007094575145,0.131904027763688,
-3.88578058618805E-16));
#17071=CARTESIAN_POINT('Ctrl Pts',(-0.107282641710421,0.110811831533068,
0.00264738937425961));
#17072=CARTESIAN_POINT('Ctrl Pts',(-0.171581760589518,0.0217576868851663,
0.0079421681227796));
#17073=CARTESIAN_POINT('Ctrl Pts',(-0.111156590520044,-0.1327225175337,
0.0158843362455596));
#17074=CARTESIAN_POINT('Ctrl Pts',(0.0512451567233008,-0.165187689797298,
0.0238265043683396));
#17075=CARTESIAN_POINT('Ctrl Pts',(0.16662620135312,-0.0465387668729445,
0.0317686724911196));
#17076=CARTESIAN_POINT('Ctrl Pts',(0.129399745666171,0.114856349193662,
0.0397108406138996));
#17077=CARTESIAN_POINT('Ctrl Pts',(-0.026390801400978,0.170972456562021,
0.0476530087366796));
#17078=CARTESIAN_POINT('Ctrl Pts',(-0.157993800025737,0.070491178324729,
0.0555951768594596));
#17079=CARTESIAN_POINT('Ctrl Pts',(-0.144863967768493,-0.0945835600760224,
0.0635373449822396));
#17080=CARTESIAN_POINT('Ctrl Pts',(0.000979154756195248,-0.17300145605975,
0.0714795131050195));
#17081=CARTESIAN_POINT('Ctrl Pts',(0.145923683802689,-0.0929367665856833,
0.0794216812277997));
#17082=CARTESIAN_POINT('Ctrl Pts',(0.157187963117837,0.0722699302633024,
0.0873638493505794));
#17083=CARTESIAN_POINT('Ctrl Pts',(0.0244514793930555,0.171268692120756,
0.0953060174733598));
#17084=CARTESIAN_POINT('Ctrl Pts',(-0.130684839550095,0.113368397534175,
0.103248185596139));
#17085=CARTESIAN_POINT('Ctrl Pts',(-0.166100541844429,-0.0483893439312075,
0.11119035371892));
#17086=CARTESIAN_POINT('Ctrl Pts',(-0.0493510193195793,-0.165817291858885,
0.119132521841699));
#17087=CARTESIAN_POINT('Ctrl Pts',(0.112609073040783,-0.131339661914923,
0.12707468996448));
#17088=CARTESIAN_POINT('Ctrl Pts',(0.17140770357293,0.0234586422209967,
0.135016858087259));
#17089=CARTESIAN_POINT('Ctrl Pts',(0.0731792588499177,0.156766393306209,
0.14295902621004));
#17090=CARTESIAN_POINT('Ctrl Pts',(-0.0920889000195865,0.146460037003638,
0.150901194332819));
#17091=CARTESIAN_POINT('Ctrl Pts',(-0.172994168426659,0.00198123296575728,
0.1588433624556));
#17092=CARTESIAN_POINT('Ctrl Pts',(-0.0954190048152776,-0.144312580095855,
0.16678553057838));
#17093=CARTESIAN_POINT('Ctrl Pts',(0.0695697692503139,-0.158401246055831,
0.17472769870116));
#17094=CARTESIAN_POINT('Ctrl Pts',(0.170825487889685,-0.0273780963649298,
0.18266986682394));
#17095=CARTESIAN_POINT('Ctrl Pts',(0.115587509852263,0.128726201683253,
0.19061203494672));
#17096=CARTESIAN_POINT('Ctrl Pts',(-0.0455405018601966,0.16690407474553,
0.198554203069499));
#17097=CARTESIAN_POINT('Ctrl Pts',(-0.164948735370872,0.0521806684752238,
0.20649637119228));
#17098=CARTESIAN_POINT('Ctrl Pts',(-0.133246981425072,-0.110345590758605,
0.214438539315059));
#17099=CARTESIAN_POINT('Ctrl Pts',(0.0205226964731592,-0.171783952668295,
0.22238070743784));
#17100=CARTESIAN_POINT('Ctrl Pts',(0.155491476033395,-0.0758505658746651,
0.230322875560619));
#17101=CARTESIAN_POINT('Ctrl Pts',(0.148014089296488,0.0895697316726553,
0.2382650436834));
#17102=CARTESIAN_POINT('Ctrl Pts',(0.00494059070111224,0.172934953166096,
0.24620721180618));
#17103=CARTESIAN_POINT('Ctrl Pts',(-0.142658996543838,0.0978739912732451,
0.25414937992896));
#17104=CARTESIAN_POINT('Ctrl Pts',(-0.159568287038446,-0.0668496016012732,
0.262091548051739));
#17105=CARTESIAN_POINT('Ctrl Pts',(-0.0302966335331915,-0.170332091689456,
0.27003371617452));
#17106=CARTESIAN_POINT('Ctrl Pts',(0.126729848780061,-0.11777288690896,
0.2779758842973));
#17107=CARTESIAN_POINT('Ctrl Pts',(0.167658770158652,0.0426783815482623,
0.28591805242008));
#17108=CARTESIAN_POINT('Ctrl Pts',(0.0549950338320791,0.164031867990689,
0.293860220542859));
#17109=CARTESIAN_POINT('Ctrl Pts',(-0.108049803339193,0.135115311719503,
0.30180238866564));
#17110=CARTESIAN_POINT('Ctrl Pts',(-0.1721099202737,-0.0175807510100837,
0.309744556788419));
#17111=CARTESIAN_POINT('Ctrl Pts',(-0.0784996687135917,-0.154171039675278,
0.3176867249112));
#17112=CARTESIAN_POINT('Ctrl Pts',(0.087024343965547,-0.14952481740522,
0.325628893033979));
#17113=CARTESIAN_POINT('Ctrl Pts',(0.172825117221703,-0.00789850112384905,
0.33357106115676));
#17114=CARTESIAN_POINT('Ctrl Pts',(0.100300328103893,0.140963653630822,
0.341513229279539));
#17115=CARTESIAN_POINT('Ctrl Pts',(-0.0641098658012952,0.160688619913292,
0.349455397402319));
#17116=CARTESIAN_POINT('Ctrl Pts',(-0.16978883637574,0.033206302186043,
0.357397565525099));
#17117=CARTESIAN_POINT('Ctrl Pts',(-0.119923789760104,-0.124696399756661,
0.36533973364788));
#17118=CARTESIAN_POINT('Ctrl Pts',(0.0398037685148125,-0.168364388974385,
0.373281901770659));
#17119=CARTESIAN_POINT('Ctrl Pts',(0.163066985633654,-0.0577933011607096,
0.38122406989344));
#17120=CARTESIAN_POINT('Ctrl Pts',(0.136944091404129,0.10572238784759,0.38916623801622));
#17121=CARTESIAN_POINT('Ctrl Pts',(-0.0146336593526265,0.172385508313924,
0.397108406138999));
#17122=CARTESIAN_POINT('Ctrl Pts',(-0.152805474769431,0.0811257933285562,
0.40505057426178));
#17123=CARTESIAN_POINT('Ctrl Pts',(-0.150991776994562,-0.0844534827151793,
0.412992742384559));
#17124=CARTESIAN_POINT('Ctrl Pts',(-0.0108540995180527,-0.172664692355881,
0.42093491050734));
#17125=CARTESIAN_POINT('Ctrl Pts',(0.139227048201004,-0.102697305280782,
0.428877078630119));
#17126=CARTESIAN_POINT('Ctrl Pts',(0.16176191642983,0.0613513639265466,
0.4368192467529));
#17127=CARTESIAN_POINT('Ctrl Pts',(0.0361062507758455,0.169195880912067,
0.444761414875679));
#17128=CARTESIAN_POINT('Ctrl Pts',(-0.12262644992489,0.12203958882886,0.45270358299846));
#17129=CARTESIAN_POINT('Ctrl Pts',(-0.169020724600573,-0.0369175042249048,
0.460645751121239));
#17130=CARTESIAN_POINT('Ctrl Pts',(-0.0605746513833496,-0.162054370729346,
0.468587919244019));
#17131=CARTESIAN_POINT('Ctrl Pts',(0.103364025571403,-0.138732785167649,
0.4765300873668));
#17132=CARTESIAN_POINT('Ctrl Pts',(0.172610636112938,0.0116822841681558,
0.484472255489579));
#17133=CARTESIAN_POINT('Ctrl Pts',(0.083728171010617,0.151395181039277,
0.49241442361236));
#17134=CARTESIAN_POINT('Ctrl Pts',(-0.081857900459256,0.152414538660527,
0.500356591735139));
#17135=CARTESIAN_POINT('Ctrl Pts',(-0.172453725526818,0.0138065207282529,
0.50829875985792));
#17136=CARTESIAN_POINT('Ctrl Pts',(-0.105064221167447,-0.137449688588867,
0.516240927980699));
#17137=CARTESIAN_POINT('Ctrl Pts',(0.0585749034388466,-0.162787862415564,
0.52418309610348));
#17138=CARTESIAN_POINT('Ctrl Pts',(0.168553398866689,-0.0389956304370821,
0.532125264226259));
#17139=CARTESIAN_POINT('Ctrl Pts',(0.124119664784058,0.120520605195094,
0.54006743234904));
#17140=CARTESIAN_POINT('Ctrl Pts',(-0.0340204335384149,0.16962758491636,
0.548009600471819));
#17141=CARTESIAN_POINT('Ctrl Pts',(-0.160994319687769,0.0633382703503284,
0.5559517685946));
#17142=CARTESIAN_POINT('Ctrl Pts',(-0.14048086942825,-0.100975406844349,
0.563893936717379));
#17143=CARTESIAN_POINT('Ctrl Pts',(0.00872748937560605,-0.172785237771916,
0.57183610484016));
#17144=CARTESIAN_POINT('Ctrl Pts',(0.149940571302356,-0.0863060399984934,
0.579778272962939));
#17145=CARTESIAN_POINT('Ctrl Pts',(0.153792685935992,0.0792383569699183,
0.58772044108572));
#17146=CARTESIAN_POINT('Ctrl Pts',(0.0167549005293281,0.17219227848818,
0.595662609208499));
#17147=CARTESIAN_POINT('Ctrl Pts',(-0.135632095058532,0.107400382926376,
0.60360477733128));
#17148=CARTESIAN_POINT('Ctrl Pts',(-0.163766157558233,-0.0557812970565469,
0.611546945454059));
#17149=CARTESIAN_POINT('Ctrl Pts',(-0.0418735953979919,-0.167861578305293,
0.61948911357684));
#17150=CARTESIAN_POINT('Ctrl Pts',(0.118379481984711,-0.126163408751231,
0.627431281699619));
#17151=CARTESIAN_POINT('Ctrl Pts',(0.17018479228316,0.0311134044783985,
0.6353734498224));
#17152=CARTESIAN_POINT('Ctrl Pts',(0.0660833491022344,0.159887142804326,
0.643315617945179));
#17153=CARTESIAN_POINT('Ctrl Pts',(-0.0985572308567358,0.142187832491218,
0.651257786067961));
#17154=CARTESIAN_POINT('Ctrl Pts',(-0.172909262181909,-0.00577013989488307,
0.659199954190738));
#17155=CARTESIAN_POINT('Ctrl Pts',(-0.0888586457050277,-0.148442071348278,
0.667142122313521));
#17156=CARTESIAN_POINT('Ctrl Pts',(0.0765956190331784,-0.155125815413241,
0.675084290436298));
#17157=CARTESIAN_POINT('Ctrl Pts',(0.171880427770071,-0.0196983758791502,
0.683026458559081));
#17158=CARTESIAN_POINT('Ctrl Pts',(0.109705106722326,0.133774799651286,
0.690968626681858));
#17159=CARTESIAN_POINT('Ctrl Pts',(-0.0529713625168984,0.164696515493808,
0.698910794804641));
#17160=CARTESIAN_POINT('Ctrl Pts',(-0.167120621735807,0.0447393032280997,
0.706852962927418));
#17161=CARTESIAN_POINT('Ctrl Pts',(-0.12817022249092,-0.116203707037801,
0.7147951310502));
#17162=CARTESIAN_POINT('Ctrl Pts',(0.0281972679828983,-0.17069218359667,
0.722737299172979));
#17163=CARTESIAN_POINT('Ctrl Pts',(0.158733164168978,-0.0688090841067,0.73067946729576));
#17164=CARTESIAN_POINT('Ctrl Pts',(0.14385317469873,0.0961102054508026,
0.738621635418538));
#17165=CARTESIAN_POINT('Ctrl Pts',(-0.00281110139369983,0.172982673038814,
0.746563803541321));
#17166=CARTESIAN_POINT('Ctrl Pts',(-0.146900119814081,0.0913852409380608,
0.754505971664098));
#17167=CARTESIAN_POINT('Ctrl Pts',(-0.156413536862055,-0.0739304602244656,
0.762448139786881));
#17168=CARTESIAN_POINT('Ctrl Pts',(-0.0226360851712103,-0.171518264656626,
0.770390307909658));
#17169=CARTESIAN_POINT('Ctrl Pts',(0.131878346029848,-0.111977717922496,
0.778332476032441));
#17170=CARTESIAN_POINT('Ctrl Pts',(0.165578663890314,0.0501459223366878,
0.786274644155218));
#17171=CARTESIAN_POINT('Ctrl Pts',(0.047591915084802,0.166330746049129,
0.794216812278001));
#17172=CARTESIAN_POINT('Ctrl Pts',(-0.113993917241593,0.130139518573781,
0.802158980400778));
#17173=CARTESIAN_POINT('Ctrl Pts',(-0.171149610334614,-0.0252728776558711,
0.81010114852356));
#17174=CARTESIAN_POINT('Ctrl Pts',(-0.0715146774936035,-0.157532721571376,
0.818043316646339));
#17175=CARTESIAN_POINT('Ctrl Pts',(0.0936350469135118,-0.14547640857611,
0.825985484769119));
#17176=CARTESIAN_POINT('Ctrl Pts',(0.173005448853992,-0.000148759965830227,
0.8339276528919));
#17177=CARTESIAN_POINT('Ctrl Pts',(0.0938850861191564,0.145315168055841,
0.841869821014678));
#17178=CARTESIAN_POINT('Ctrl Pts',(-0.0712436606821878,0.157655473343934,
0.849811989137461));
#17179=CARTESIAN_POINT('Ctrl Pts',(-0.171105895159299,0.0255671684868261,
0.857754157260238));
#17180=CARTESIAN_POINT('Ctrl Pts',(-0.114217551294,-0.129943289319231,0.86569632538302));
#17181=CARTESIAN_POINT('Ctrl Pts',(0.0473058035714782,-0.166412344527548,
0.873638493505798));
#17182=CARTESIAN_POINT('Ctrl Pts',(0.16549218245563,-0.0504305959589149,
0.88158066162858));
#17183=CARTESIAN_POINT('Ctrl Pts',(0.132070720552549,0.111750759440056,
0.889522829751358));
#17184=CARTESIAN_POINT('Ctrl Pts',(-0.022341089517305,0.171556938600217,
0.89746499787414));
#17185=CARTESIAN_POINT('Ctrl Pts',(-0.156286166401977,0.074199337288632,
0.905407165996919));
#17186=CARTESIAN_POINT('Ctrl Pts',(-0.147057058974526,-0.0911324797668838,
0.913349334119699));
#17187=CARTESIAN_POINT('Ctrl Pts',(-0.00310857778072832,-0.172977582960567,
0.92129150224248));
#17188=CARTESIAN_POINT('Ctrl Pts',(0.143687680016546,-0.0963574495000853,
0.929233670365259));
#17189=CARTESIAN_POINT('Ctrl Pts',(0.158851261322436,0.0685360068793772,
0.93717583848804));
#17190=CARTESIAN_POINT('Ctrl Pts',(0.0284907678468484,0.170643439985825,
0.945118006610819));
#17191=CARTESIAN_POINT('Ctrl Pts',(-0.127970195944242,0.116423951198588,
0.9530601747336));
#17192=CARTESIAN_POINT('Ctrl Pts',(-0.167197313372666,-0.0444518375735043,
0.961002342856378));
#17193=CARTESIAN_POINT('Ctrl Pts',(-0.0532545149190986,-0.164605176417482,
0.96894451097916));
#17194=CARTESIAN_POINT('Ctrl Pts',(0.10947489024455,-0.133963263130763,
0.976886679101939));
#17195=CARTESIAN_POINT('Ctrl Pts',(0.1719140491614,0.0194027617526574,0.984828847224719));
#17196=CARTESIAN_POINT('Ctrl Pts',(0.0768622776450996,0.154993863549195,
0.992771015347499));
#17197=CARTESIAN_POINT('Ctrl Pts',(-0.088603236555915,0.148594663210074,
1.00071318347028));
#17198=CARTESIAN_POINT('Ctrl Pts',(-0.172899083515371,0.00606748566075909,
1.00865535159306));
#17199=CARTESIAN_POINT('Ctrl Pts',(-0.0988016073770141,-0.142018132090297,
1.01659751971584));
#17200=CARTESIAN_POINT('Ctrl Pts',(0.0658082913934689,-0.160000550769587,
1.02453968783862));
#17201=CARTESIAN_POINT('Ctrl Pts',(0.170131034504888,-0.0314060274628177,
1.0324818559614));
#17202=CARTESIAN_POINT('Ctrl Pts',(0.118596271784576,0.125959643463681,
1.04042402408418));
#17203=CARTESIAN_POINT('Ctrl Pts',(-0.0415848597483297,0.167933340651612,
1.04836619220696));
#17204=CARTESIAN_POINT('Ctrl Pts',(-0.163669987576804,0.0560628453550813,
1.05630836032974));
#17205=CARTESIAN_POINT('Ctrl Pts',(-0.135816592328243,-0.107166975841641,
1.06425052845252));
#17206=CARTESIAN_POINT('Ctrl Pts',(0.0164587544616562,-0.172220837485682,
1.0721926965753));
#17207=CARTESIAN_POINT('Ctrl Pts',(0.153656191292587,-0.0795027190739688,
1.08013486469808));
#17208=CARTESIAN_POINT('Ctrl Pts',(0.150088771199207,0.0860480576341552,
1.08807703282086));
#17209=CARTESIAN_POINT('Ctrl Pts',(0.00902461748204118,0.172769973496559,
1.09601920094364));
#17210=CARTESIAN_POINT('Ctrl Pts',(-0.140307012982855,0.101216844302358,
1.10396136906642));
#17211=CARTESIAN_POINT('Ctrl Pts',(-0.161103005268346,-0.0630613126743013,
1.1119035371892));
#17212=CARTESIAN_POINT('Ctrl Pts',(-0.0343120939874615,-0.1695688287065,
1.11984570531198));
#17213=CARTESIAN_POINT('Ctrl Pts',(0.123912220401285,-0.120733877175888,
1.12778787343476));
#17214=CARTESIAN_POINT('Ctrl Pts',(0.168620210916381,0.0387057093103061,
1.13573004155754));
#17215=CARTESIAN_POINT('Ctrl Pts',(0.0588547652196237,0.162686889679659,
1.14367220968032));
#17216=CARTESIAN_POINT('Ctrl Pts',(-0.104827691798069,0.137630165643247,
1.1516143778031));
#17217=CARTESIAN_POINT('Ctrl Pts',(-0.172477213770776,-0.0135099294065116,
1.15955654592588));
#17218=CARTESIAN_POINT('Ctrl Pts',(-0.0821198886720452,-0.152273541192125,
1.16749871404866));
#17219=CARTESIAN_POINT('Ctrl Pts',(0.083467690946984,-0.15153894559049,
1.17544088217144));
#17220=CARTESIAN_POINT('Ctrl Pts',(0.172590290696882,-0.0119791076405788,
1.18338305029422));
#17221=CARTESIAN_POINT('Ctrl Pts',(0.103602453294194,0.13855482356859,1.191325218417));
#17222=CARTESIAN_POINT('Ctrl Pts',(-0.0602958748103966,0.162158302111078,
1.19926738653978));
#17223=CARTESIAN_POINT('Ctrl Pts',(-0.168956987158091,0.0372081167644847,
1.20720955466256));
#17224=CARTESIAN_POINT('Ctrl Pts',(-0.122836141658186,-0.121828526073448,
1.21515172278534));
#17225=CARTESIAN_POINT('Ctrl Pts',(0.0358152290369173,-0.169257723108079,
1.22309389090812));
#17226=CARTESIAN_POINT('Ctrl Pts',(0.161656170495932,-0.0616294572691503,
1.2310360590309));
#17227=CARTESIAN_POINT('Ctrl Pts',(0.13940345221127,0.102457722863032,1.23897822715368));
#17228=CARTESIAN_POINT('Ctrl Pts',(-0.0105571497596809,0.172683102970871,
1.24692039527646));
#17229=CARTESIAN_POINT('Ctrl Pts',(-0.150846317973597,0.0847130203482025,
1.25486256339924));
#17230=CARTESIAN_POINT('Ctrl Pts',(-0.152944761892581,-0.0808628918127005,
1.26280473152202));
#17231=CARTESIAN_POINT('Ctrl Pts',(-0.0149300913057054,-0.172360087712588,
1.2707468996448));
#17232=CARTESIAN_POINT('Ctrl Pts',(0.136762076743997,-0.105957736043287,
1.27868906776758));
#17233=CARTESIAN_POINT('Ctrl Pts',(0.163166132393764,0.0575127872937276,
1.28663123589036));
#17234=CARTESIAN_POINT('Ctrl Pts',(0.0400932480780463,0.168295688956082,
1.29457340401314));
#17235=CARTESIAN_POINT('Ctrl Pts',(-0.119709170414695,0.124902449862528,
1.30251557213592));
#17236=CARTESIAN_POINT('Ctrl Pts',(-0.169845690614082,-0.0329142650230248,
1.3104577402587));
#17237=CARTESIAN_POINT('Ctrl Pts',(-0.0643861093061943,-0.160578131733314,
1.31839990838148));
#17238=CARTESIAN_POINT('Ctrl Pts',(0.100057762773863,-0.141135932963798,
1.32634207650426));
#17239=CARTESIAN_POINT('Ctrl Pts',(0.172838444806952,0.00760127985757451,
1.33428424462704));
#17240=CARTESIAN_POINT('Ctrl Pts',(0.0872813550697656,0.149374939398002,
1.34222641274982));
#17241=CARTESIAN_POINT('Ctrl Pts',(-0.0782344227434143,0.154305808621531,
1.3501685808726));
#17242=CARTESIAN_POINT('Ctrl Pts',(-0.172079431848303,0.0178767046294837,
1.35811074899538));
#17243=CARTESIAN_POINT('Ctrl Pts',(-0.108282003268856,-0.134929297194493,
1.36605291711816));
#17244=CARTESIAN_POINT('Ctrl Pts',(0.0547128650701426,-0.164126201264144,
1.37399508524094));
#17245=CARTESIAN_POINT('Ctrl Pts',(0.167585127127835,-0.0429666431014547,
1.38193725336372));
#17246=CARTESIAN_POINT('Ctrl Pts',(0.126932197981417,0.117554773230619,
1.3898794214865));
#17247=CARTESIAN_POINT('Ctrl Pts',(-0.0300036684000219,0.170383942402052,
1.39782158960928));
#17248=CARTESIAN_POINT('Ctrl Pts',(-0.159453085214751,0.0671239123677834,
1.40576375773206));
#17249=CARTESIAN_POINT('Ctrl Pts',(-0.142827107870127,-0.0976285101620078,
1.41370592585484));
#17250=CARTESIAN_POINT('Ctrl Pts',(0.00464319840846943,-0.172943201171859,
1.42164809397762));
#17251=CARTESIAN_POINT('Ctrl Pts',(0.147859810582222,-0.0898241270588577,
1.4295902621004));
#17252=CARTESIAN_POINT('Ctrl Pts',(0.155621735944117,0.0755830265922534,
1.43753243022318));
#17253=CARTESIAN_POINT('Ctrl Pts',(0.0208179928734729,0.171748455656582,
1.44547459834596));
#17254=CARTESIAN_POINT('Ctrl Pts',(-0.133056846329205,0.11057447892796,
1.45341676646874));
#17255=CARTESIAN_POINT('Ctrl Pts',(-0.165038560097216,-0.0518967460486161,
1.46135893459152));
#17256=CARTESIAN_POINT('Ctrl Pts',(-0.0458268296361176,-0.166825854601292,
1.4693011027143));
#17257=CARTESIAN_POINT('Ctrl Pts',(0.115364766925686,-0.128924136976022,
1.47724327083708));
#17258=CARTESIAN_POINT('Ctrl Pts',(0.170874595884426,0.0270830477535184,
1.48518543895986));
#17259=CARTESIAN_POINT('Ctrl Pts',(0.0698377457337486,0.158283721017069,
1.49312760708264));
#17260=CARTESIAN_POINT('Ctrl Pts',(-0.0951624750893037,0.144471999488883,
1.50106977520542));
#17261=CARTESIAN_POINT('Ctrl Pts',(-0.173012914651864,-0.00167525885548286,
1.5090119433282));
#17262=CARTESIAN_POINT('Ctrl Pts',(-0.092311001583214,-0.14631755460685,
1.51695411145098));
#17263=CARTESIAN_POINT('Ctrl Pts',(0.072853104778531,-0.156861289272697,
1.52489627957376));
#17264=CARTESIAN_POINT('Ctrl Pts',(0.171475934783304,-0.0238129810547936,
1.53283844769654));
#17265=CARTESIAN_POINT('Ctrl Pts',(0.11261423476106,0.131269690464983,1.54078061581932));
#17266=CARTESIAN_POINT('Ctrl Pts',(0.00518264413773371,0.154149172621267,
1.54607539456784));
#17267=CARTESIAN_POINT('Ctrl Pts',(-0.0415060733757155,0.140340900570467,
1.5487227839421));
#17268=CARTESIAN_POINT('Ctrl Pts',(-0.146248097568756,-0.000123763188177425,
1.45893449541571));
#17269=CARTESIAN_POINT('Ctrl Pts',(-0.146367493381718,-0.0150081347743067,
1.45974264180765));
#17270=CARTESIAN_POINT('Ctrl Pts',(-0.144277648885518,-0.0298597803798721,
1.46055078819958));
#17271=CARTESIAN_POINT('Ctrl Pts',(-0.139839652725699,-0.043973059977961,
1.46135893459152));
#17272=CARTESIAN_POINT('Ctrl Pts',(-0.125301316610186,-0.0902064488995044,
1.46400632396578));
#17273=CARTESIAN_POINT('Ctrl Pts',(-0.08556407312315,-0.1285161517504,1.46665371334004));
#17274=CARTESIAN_POINT('Ctrl Pts',(-0.0388301852859989,-0.141354050238301,
1.4693011027143));
#17275=CARTESIAN_POINT('Ctrl Pts',(0.00790370255115092,-0.154191948726202,
1.47194849208856));
#17276=CARTESIAN_POINT('Ctrl Pts',(0.0616342347384179,-0.141558042851112,
1.47459588146282));
#17277=CARTESIAN_POINT('Ctrl Pts',(0.0977511389918415,-0.109239892458645,
1.47724327083708));
#17278=CARTESIAN_POINT('Ctrl Pts',(0.133868043245265,-0.0769217420661769,
1.47989066021134));
#17279=CARTESIAN_POINT('Ctrl Pts',(0.152371319564846,-0.024919347156331,
1.4825380495856));
#17280=CARTESIAN_POINT('Ctrl Pts',(0.144783482699524,0.0229486291758506,
1.48518543895986));
#17281=CARTESIAN_POINT('Ctrl Pts',(0.137195645834202,0.0708166055080336,
1.48783282833412));
#17282=CARTESIAN_POINT('Ctrl Pts',(0.103516695783975,0.114550163262552,
1.49048021770838));
#17283=CARTESIAN_POINT('Ctrl Pts',(0.0591771839550196,0.13411498855178,
1.49312760708264));
#17284=CARTESIAN_POINT('Ctrl Pts',(0.014837672126065,0.153679813841007,
1.4957749964569));
#17285=CARTESIAN_POINT('Ctrl Pts',(-0.0401624014816186,0.149075906664945,
1.49842238583116));
#17286=CARTESIAN_POINT('Ctrl Pts',(-0.0806375115458872,0.122416076686187,
1.50106977520542));
#17287=CARTESIAN_POINT('Ctrl Pts',(-0.0937869288003098,0.113754921033589,
1.50192985013695));
#17288=CARTESIAN_POINT('Ctrl Pts',(-0.105403311347291,0.102765876910903,
1.50278992506847));
#17289=CARTESIAN_POINT('Ctrl Pts',(-0.115078604842433,0.0902138214954038,
1.50365));
#17290=CARTESIAN_POINT('Ctrl Pts',(-0.0686146973663081,-0.0959584553529135,
1.07336015076065E-17));
#17291=CARTESIAN_POINT('Ctrl Pts',(-0.0712979561985307,-0.0944995001033786,
9.02613639135873E-18));
#17292=CARTESIAN_POINT('Ctrl Pts',(-0.0739152333025289,-0.0929325179580126,
1.64107321374712E-17));
#17293=CARTESIAN_POINT('Ctrl Pts',(-0.0764591723283171,-0.0912589988675934,
1.6154612370034E-17));
#17294=CARTESIAN_POINT('Ctrl Pts',(-0.0824897891353913,-0.0872917841461184,
1.52077426268717E-17));
#17295=CARTESIAN_POINT('Ctrl Pts',(-0.0881090519769445,-0.0827275518978924,
1.30971627060498E-17));
#17296=CARTESIAN_POINT('Ctrl Pts',(-0.0932912133381108,-0.0776621329443405,
1.43114686768087E-17));
#17297=CARTESIAN_POINT('Ctrl Pts',(-0.0960634919631888,-0.074952307504085,
1.49610807310118E-17));
#17298=CARTESIAN_POINT('Ctrl Pts',(-0.0987043519497191,-0.0721043812799658,
1.74993329480528E-17));
#17299=CARTESIAN_POINT('Ctrl Pts',(-0.101206237074718,-0.0691378820326018,
9.97465998686664E-18));
#17300=CARTESIAN_POINT('Ctrl Pts',(-0.105823426721714,-0.0636632543305198,
-3.91200561030858E-18));
#17301=CARTESIAN_POINT('Ctrl Pts',(-0.109972666997065,-0.0577811896139199,
2.24798207762934E-18));
#17302=CARTESIAN_POINT('Ctrl Pts',(-0.113625452403263,-0.0515741981665521,
9.54097911787244E-18));
#17303=CARTESIAN_POINT('Ctrl Pts',(-0.115386295340069,-0.0485820878086944,
1.30566037435822E-17));
#17304=CARTESIAN_POINT('Ctrl Pts',(-0.117027309103105,-0.0455212415157476,
-2.79521757168051E-18));
#17305=CARTESIAN_POINT('Ctrl Pts',(-0.118543833519887,-0.0424058589801268,
-3.46944695195361E-18));
#17306=CARTESIAN_POINT('Ctrl Pts',(-0.122700941917732,-0.0338659484069709,
-5.31764971597768E-18));
#17307=CARTESIAN_POINT('Ctrl Pts',(-0.125931492798984,-0.0249085743588085,
-1.15219401683824E-18));
#17308=CARTESIAN_POINT('Ctrl Pts',(-0.128167520083254,-0.0157105262534848,
9.54097911787244E-18));
#17309=CARTESIAN_POINT('Ctrl Pts',(-0.128992166906242,-0.0123182862745252,
1.3484621181291E-17));
#17310=CARTESIAN_POINT('Ctrl Pts',(-0.129681150280034,-0.00889298553317688,
1.10989611676181E-17));
#17311=CARTESIAN_POINT('Ctrl Pts',(-0.130229483957028,-0.00544263935519351,
9.54097911787244E-18));
#17312=CARTESIAN_POINT('Ctrl Pts',(-0.130761899349706,-0.00209245771889707,
8.02822573502553E-18));
#17313=CARTESIAN_POINT('Ctrl Pts',(-0.131160261982709,0.00127366115726457,
1.11791151702242E-17));
#17314=CARTESIAN_POINT('Ctrl Pts',(-0.131420990891747,0.00464012593483382,
8.67361737988404E-18));
#17315=CARTESIAN_POINT('Ctrl Pts',(-0.131728666658755,0.00861275649723166,
5.71697955546795E-18));
#17316=CARTESIAN_POINT('Ctrl Pts',(-0.131845259942619,0.0125891451047215,
-9.26473565962443E-18));
#17317=CARTESIAN_POINT('Ctrl Pts',(-0.131765781147177,0.0165567997877194,
-1.04083408558608E-17));
#17318=CARTESIAN_POINT('Ctrl Pts',(-0.131635692412819,0.0230509492424239,
-1.21888544026837E-17));
#17319=CARTESIAN_POINT('Ctrl Pts',(-0.13098103789945,0.0295216962360144,
-2.67049856555875E-17));
#17320=CARTESIAN_POINT('Ctrl Pts',(-0.129839098367345,0.0359278479980343,
-3.46944695195361E-17));
#17321=CARTESIAN_POINT('Ctrl Pts',(-0.129254890951344,0.0392051855997028,
-3.87818275556788E-17));
#17322=CARTESIAN_POINT('Ctrl Pts',(-0.128542951403208,0.0424656461998481,
-3.10678831811161E-17));
#17323=CARTESIAN_POINT('Ctrl Pts',(-0.1277070993652,0.0457037274559979,
-3.29597460435593E-17));
#17324=CARTESIAN_POINT('Ctrl Pts',(-0.126886363095037,0.0488832504000222,
-3.48173959609792E-17));
#17325=CARTESIAN_POINT('Ctrl Pts',(-0.125948031872817,0.0520333657183593,
-3.53366201082739E-17));
#17326=CARTESIAN_POINT('Ctrl Pts',(-0.124899042599898,0.0551436241923499,
-3.46944695195361E-17));
#17327=CARTESIAN_POINT('Ctrl Pts',(-0.122234979928128,0.0630425834229368,
-3.30636335736642E-17));
#17328=CARTESIAN_POINT('Ctrl Pts',(-0.118856305871375,0.070695441500891,
-2.1366080483524E-17));
#17329=CARTESIAN_POINT('Ctrl Pts',(-0.114834854776346,0.078019637496205,
-1.73472347597681E-17));
#17330=CARTESIAN_POINT('Ctrl Pts',(-0.11215901866562,0.0828930893082948,
-1.46731322388254E-17));
#17331=CARTESIAN_POINT('Ctrl Pts',(-0.109198005187061,0.0876211033078822,
8.28606628989234E-18));
#17332=CARTESIAN_POINT('Ctrl Pts',(-0.105966883726074,0.0921780034666525,
8.67361737988404E-18));
#17333=CARTESIAN_POINT('Ctrl Pts',(-0.104137243112614,0.094758373688769,
8.89307035390601E-18));
#17334=CARTESIAN_POINT('Ctrl Pts',(-0.102221042121924,0.0972831505018574,
-2.31209379389524E-17));
#17335=CARTESIAN_POINT('Ctrl Pts',(-0.100229777791505,0.0997373632832089,
-2.08166817117217E-17));
#17336=CARTESIAN_POINT('Ctrl Pts',(-0.0937202782075859,0.107760254486057,
-1.32840027382311E-17));
#17337=CARTESIAN_POINT('Ctrl Pts',(-0.0863914655699752,0.115060936709644,
5.4842312373535E-18));
#17338=CARTESIAN_POINT('Ctrl Pts',(-0.0783508402622743,0.121487309774744,
1.38777878078145E-17));
#17339=CARTESIAN_POINT('Ctrl Pts',(-0.073610711791116,0.125275800441382,
1.8825977152717E-17));
#17340=CARTESIAN_POINT('Ctrl Pts',(-0.068622257850438,0.128760167547443,
-9.09579695168528E-18));
#17341=CARTESIAN_POINT('Ctrl Pts',(-0.0634007094575209,0.131904027763685,
-6.93889390390723E-18));
#17342=CARTESIAN_POINT('Origin',(0.,0.,0.));
#17343=CARTESIAN_POINT('Origin',(-0.0721687836487033,-0.125,-0.3));
#17344=CARTESIAN_POINT('',(-0.0721687836487033,-0.125,-0.3));
#17345=CARTESIAN_POINT('',(0.0721687836487032,-0.125,-0.3));
#17346=CARTESIAN_POINT('',(-0.0360843918243517,-0.125,-0.3));
#17347=CARTESIAN_POINT('',(-0.0721687836487033,-0.125,-0.15));
#17348=CARTESIAN_POINT('',(-0.0721687836487033,-0.125,-0.3));
#17349=CARTESIAN_POINT('',(0.0721687836487032,-0.125,-0.15));
#17350=CARTESIAN_POINT('',(-0.0721687836487033,-0.125,-0.15));
#17351=CARTESIAN_POINT('',(0.0721687836487032,-0.125,-0.3));
#17352=CARTESIAN_POINT('Origin',(-0.144337567297406,1.76762539787485E-17,
-0.3));
#17353=CARTESIAN_POINT('',(-0.144337567297406,1.76762539787485E-17,-0.3));
#17354=CARTESIAN_POINT('',(-0.126295371385231,-0.03125,-0.3));
#17355=CARTESIAN_POINT('',(-0.144337567297406,2.77555756156289E-17,-0.15));
#17356=CARTESIAN_POINT('',(-0.144337567297406,1.76762539787485E-17,-0.3));
#17357=CARTESIAN_POINT('',(-0.144337567297406,1.76762539787485E-17,-0.15));
#17358=CARTESIAN_POINT('Origin',(-0.0721687836487032,0.125,-0.3));
#17359=CARTESIAN_POINT('',(-0.0721687836487032,0.125,-0.3));
#17360=CARTESIAN_POINT('',(-0.090210979560879,0.09375,-0.3));
#17361=CARTESIAN_POINT('',(-0.0721687836487032,0.125,-0.15));
#17362=CARTESIAN_POINT('',(-0.0721687836487032,0.125,-0.3));
#17363=CARTESIAN_POINT('',(-0.0721687836487032,0.125,-0.15));
#17364=CARTESIAN_POINT('Origin',(0.0721687836487032,0.125,-0.3));
#17365=CARTESIAN_POINT('',(0.0721687836487032,0.125,-0.3));
#17366=CARTESIAN_POINT('',(0.0360843918243516,0.125,-0.3));
#17367=CARTESIAN_POINT('',(0.0721687836487032,0.125,-0.15));
#17368=CARTESIAN_POINT('',(0.0721687836487032,0.125,-0.3));
#17369=CARTESIAN_POINT('',(0.0721687836487032,0.125,-0.15));
#17370=CARTESIAN_POINT('Origin',(0.144337567297406,0.,-0.3));
#17371=CARTESIAN_POINT('',(0.144337567297406,0.,-0.3));
#17372=CARTESIAN_POINT('',(0.126295371385231,0.03125,-0.3));
#17373=CARTESIAN_POINT('',(0.144337567297406,0.,-0.15));
#17374=CARTESIAN_POINT('',(0.144337567297406,0.,-0.3));
#17375=CARTESIAN_POINT('',(0.144337567297406,0.,-0.15));
#17376=CARTESIAN_POINT('Origin',(0.0721687836487032,-0.125,-0.3));
#17377=CARTESIAN_POINT('',(0.0902109795608791,-0.09375,-0.3));
#17378=CARTESIAN_POINT('',(0.0721687836487032,-0.125,-0.15));
#17379=CARTESIAN_POINT('Origin',(0.,0.,-0.15));
#17380=CARTESIAN_POINT('Origin',(0.,0.,0.));
#17381=CARTESIAN_POINT('',(-0.275,-3.36777869765522E-17,0.));
#17382=CARTESIAN_POINT('Origin',(0.,0.,0.));
#17383=CARTESIAN_POINT('Origin',(0.,0.,-0.3));
#17384=CARTESIAN_POINT('',(-0.275,-3.36777869765522E-17,-0.3));
#17385=CARTESIAN_POINT('',(-0.275,-3.36777869765522E-17,-0.3));
#17386=CARTESIAN_POINT('Origin',(0.,0.,-0.3));
#17387=CARTESIAN_POINT('Origin',(0.,0.,-0.3));
#17388=CARTESIAN_POINT('Origin',(0.,0.,1.6));
#17389=CARTESIAN_POINT('',(0.,0.,0.));
#17390=CARTESIAN_POINT('Origin',(0.,0.,0.12));
#17391=CARTESIAN_POINT('',(-0.12639138516214,8.91322620741042E-5,0.00934196736194174));
#17392=CARTESIAN_POINT('',(-0.12645,1.54856587752183E-17,-5.55111512312578E-17));
#17393=CARTESIAN_POINT('',(-0.12645,1.54856587752183E-17,0.12));
#17394=CARTESIAN_POINT('',(-0.0488748409397564,0.116622692573588,0.));
#17395=CARTESIAN_POINT('Origin',(0.,0.,0.));
#17396=CARTESIAN_POINT('Ctrl Pts',(-0.0489111879062984,0.116810626195002,
1.20007714660797E-17));
#17397=CARTESIAN_POINT('Ctrl Pts',(-0.0838963038512042,0.101957324585112,
0.00240024091002088));
#17398=CARTESIAN_POINT('Ctrl Pts',(-0.11198221847721,0.0702793053867637,
0.00480048182004174));
#17399=CARTESIAN_POINT('Ctrl Pts',(-0.122072221370749,0.0336561163696377,
0.00720072273006261));
#17400=CARTESIAN_POINT('Ctrl Pts',(-0.125072637487486,0.022765653033531,
0.00791447094068899));
#17401=CARTESIAN_POINT('Ctrl Pts',(-0.126481745582665,0.0114379076904012,
0.00862821915131536));
#17402=CARTESIAN_POINT('Ctrl Pts',(-0.12639138516214,8.91322620741042E-5,
0.00934196736194174));
#17403=CARTESIAN_POINT('Origin',(0.,0.,0.12));
#17404=CARTESIAN_POINT('',(-0.126396145829628,-9.95859796292312E-5,0.0593419673619417));
#17405=CARTESIAN_POINT('',(-0.126575671592806,-7.20628672610732E-5,0.0456580326380584));
#17406=CARTESIAN_POINT('',(-0.12645,1.54856587752183E-17,0.12));
#17407=CARTESIAN_POINT('',(-0.10808967569503,-0.0656218295092665,0.));
#17408=CARTESIAN_POINT('Ctrl Pts',(-0.126575671592806,-7.20628672610732E-5,
0.0456580326380584));
#17409=CARTESIAN_POINT('Ctrl Pts',(-0.126327459688109,0.0361497101693465,
0.0433719816070355));
#17410=CARTESIAN_POINT('Ctrl Pts',(-0.109912066394173,0.0725710138228805,
0.0410859305760125));
#17411=CARTESIAN_POINT('Ctrl Pts',(-0.0824515099939393,0.0961223418729112,
0.0387998795449896));
#17412=CARTESIAN_POINT('Ctrl Pts',(-0.05137998778939,0.122770586059505,
0.036213220908657));
#17413=CARTESIAN_POINT('Ctrl Pts',(-0.00616751748104999,0.132941603485868,
0.0336265622723243));
#17414=CARTESIAN_POINT('Ctrl Pts',(0.0333172074018229,0.122176268745047,
0.0310399036359917));
#17415=CARTESIAN_POINT('Ctrl Pts',(0.0728019322846963,0.111410934004226,
0.028453244999659));
#17416=CARTESIAN_POINT('Ctrl Pts',(0.106558911742102,0.0797092470962188,
0.0258665863633264));
#17417=CARTESIAN_POINT('Ctrl Pts',(0.11981357554495,0.0409763259700822,
0.0232799277269937));
#17418=CARTESIAN_POINT('Ctrl Pts',(0.133068239347797,0.00224340484394604,
0.0206932690906611));
#17419=CARTESIAN_POINT('Ctrl Pts',(0.125820587496086,-0.0435207505003201,
0.0181066104543285));
#17420=CARTESIAN_POINT('Ctrl Pts',(0.101166903546451,-0.0762076816581678,
0.0155199518179958));
#17421=CARTESIAN_POINT('Ctrl Pts',(0.0765132195968157,-0.108894612816016,
0.0129332931816632));
#17422=CARTESIAN_POINT('Ctrl Pts',(0.0344535035492562,-0.128504319787445,
0.0103466345453306));
#17423=CARTESIAN_POINT('Ctrl Pts',(-0.00636464094143544,-0.126469737202777,
0.00775997590899791));
#17424=CARTESIAN_POINT('Ctrl Pts',(-0.0471827854321269,-0.124435154618108,
0.00517331727266527));
#17425=CARTESIAN_POINT('Ctrl Pts',(-0.0867593583659505,-0.100756282477341,
0.00258665863633259));
#17426=CARTESIAN_POINT('Ctrl Pts',(-0.108089675695031,-0.0656218295092657,
-5.55111512312578E-17));
#17427=CARTESIAN_POINT('Origin',(0.,0.,0.));
#17428=CARTESIAN_POINT('Ctrl Pts',(-0.12639138516214,8.91322620741042E-5,
0.00934196736194174));
#17429=CARTESIAN_POINT('Ctrl Pts',(-0.126154274972366,-0.0296906128949183,
0.011214877787648));
#17430=CARTESIAN_POINT('Ctrl Pts',(-0.115592373032178,-0.0596151635265703,
0.0130877882133543));
#17431=CARTESIAN_POINT('Ctrl Pts',(-0.0963650578556872,-0.0821635787359664,
0.0149606986390606));
#17432=CARTESIAN_POINT('Ctrl Pts',(-0.0698103971670931,-0.113304978845907,
0.0175473572753932));
#17433=CARTESIAN_POINT('Ctrl Pts',(-0.0267272342632827,-0.130377059081323,
0.0201340159117258));
#17434=CARTESIAN_POINT('Ctrl Pts',(0.0139574509341311,-0.125868770046104,
0.0227206745480584));
#17435=CARTESIAN_POINT('Ctrl Pts',(0.0546421361315456,-0.121360481010885,
0.0253073331843911));
#17436=CARTESIAN_POINT('Ctrl Pts',(0.0929283436225635,-0.0952718227050311,
0.0278939918207237));
#17437=CARTESIAN_POINT('Ctrl Pts',(0.112018291148455,-0.0590635258734944,
0.0304806504570564));
#17438=CARTESIAN_POINT('Ctrl Pts',(0.131108238674346,-0.0228552290419586,
0.033067309093389));
#17439=CARTESIAN_POINT('Ctrl Pts',(0.131001926235112,0.0234727063152593,
0.0356539677297216));
#17440=CARTESIAN_POINT('Ctrl Pts',(0.111741771403992,0.0595891814911641,
0.0382406263660542));
#17441=CARTESIAN_POINT('Ctrl Pts',(0.0924816165728724,0.0957056566670696,
0.0408272850023869));
#17442=CARTESIAN_POINT('Ctrl Pts',(0.0540676193498672,0.121610671661662,
0.0434139436387195));
#17443=CARTESIAN_POINT('Ctrl Pts',(0.0133639835211523,0.125930636937597,
0.0460006022750522));
#17444=CARTESIAN_POINT('Ctrl Pts',(-0.0273396523075625,0.130250602213533,
0.0485872609113848));
#17445=CARTESIAN_POINT('Ctrl Pts',(-0.0703329267419868,0.112985517770812,
0.0511739195477175));
#17446=CARTESIAN_POINT('Ctrl Pts',(-0.0967449447385466,0.0817152626609385,
0.0537605781840501));
#17447=CARTESIAN_POINT('Ctrl Pts',(-0.115741878896724,0.0592240248649833,
0.0556210412433473));
#17448=CARTESIAN_POINT('Ctrl Pts',(-0.126160906676814,0.0294875554882879,
0.0574815043026445));
#17449=CARTESIAN_POINT('Ctrl Pts',(-0.126396145829628,-9.95859796292312E-5,
0.0593419673619417));
#17450=CARTESIAN_POINT('Origin',(0.,0.,0.12));
#17451=CARTESIAN_POINT('',(-0.126529791093031,9.025049583615E-5,0.109341967361942));
#17452=CARTESIAN_POINT('',(-0.126349242904067,8.85860673823967E-5,0.0956580326380584));
#17453=CARTESIAN_POINT('',(-0.12645,1.54856587752183E-17,0.12));
#17454=CARTESIAN_POINT('Ctrl Pts',(-0.126349242904067,8.85860673823967E-5,
0.0956580326380584));
#17455=CARTESIAN_POINT('Ctrl Pts',(-0.126441591528965,0.0135570965972842,
0.0948119253946973));
#17456=CARTESIAN_POINT('Ctrl Pts',(-0.124448136217638,0.0269990101701626,
0.0939658181513361));
#17457=CARTESIAN_POINT('Ctrl Pts',(-0.120249444863787,0.0397126388809939,
0.093119710907975));
#17458=CARTESIAN_POINT('Ctrl Pts',(-0.107413505522824,0.0785798365820317,
0.0905330522716423));
#17459=CARTESIAN_POINT('Ctrl Pts',(-0.0739673525896496,0.110640458354997,
0.0879463936353097));
#17460=CARTESIAN_POINT('Ctrl Pts',(-0.0345920580258737,0.121821308595361,
0.085359734998977));
#17461=CARTESIAN_POINT('Ctrl Pts',(0.00478323653790218,0.133002158835724,
0.0827730763626444));
#17462=CARTESIAN_POINT('Ctrl Pts',(0.0500876727322792,0.123303237543486,
0.0801864177263117));
#17463=CARTESIAN_POINT('Ctrl Pts',(0.0814342209129887,0.0969820390626645,
0.077599759089979));
#17464=CARTESIAN_POINT('Ctrl Pts',(0.112780769093698,0.0706608405818426,
0.0750131004536464));
#17465=CARTESIAN_POINT('Ctrl Pts',(0.13016942926074,0.0277173649124373,
0.0724264418173139));
#17466=CARTESIAN_POINT('Ctrl Pts',(0.12596827751407,-0.0129984006283456,
0.0698397831809812));
#17467=CARTESIAN_POINT('Ctrl Pts',(0.121767125767399,-0.0537141661691284,
0.0672531245446486));
#17468=CARTESIAN_POINT('Ctrl Pts',(0.0959761621070158,-0.0922022215812886,
0.0646664659083159));
#17469=CARTESIAN_POINT('Ctrl Pts',(0.059914723710966,-0.111567668284471,
0.0620798072719833));
#17470=CARTESIAN_POINT('Ctrl Pts',(0.0238532853149157,-0.130933114987654,
0.0594931486356506));
#17471=CARTESIAN_POINT('Ctrl Pts',(-0.0224786278168013,-0.131175952981858,
0.056906489999318));
#17472=CARTESIAN_POINT('Ctrl Pts',(-0.0587401909579078,-0.112190380850839,
0.0543198313629853));
#17473=CARTESIAN_POINT('Ctrl Pts',(-0.0950017540990138,-0.0932048087198191,
0.0517331727266527));
#17474=CARTESIAN_POINT('Ctrl Pts',(-0.12119296724951,-0.0549908264635757,
0.0491465140903201));
#17475=CARTESIAN_POINT('Ctrl Pts',(-0.125823286774378,-0.0143210998620416,
0.0465598554539874));
#17476=CARTESIAN_POINT('Ctrl Pts',(-0.126361397696569,-0.0095946821776348,
0.0462592478486778));
#17477=CARTESIAN_POINT('Ctrl Pts',(-0.12660831057823,-0.00483509759607578,
0.0459586402433681));
#17478=CARTESIAN_POINT('Ctrl Pts',(-0.126575671592806,-7.20628672610732E-5,
0.0456580326380584));
#17479=CARTESIAN_POINT('Ctrl Pts',(-0.126396145829628,-9.95859796292312E-5,
0.0593419673619417));
#17480=CARTESIAN_POINT('Ctrl Pts',(-0.12648796685852,-0.0116483513064931,
0.0600681629389771));
#17481=CARTESIAN_POINT('Ctrl Pts',(-0.125028206814926,-0.0231743653405588,
0.0607943585160125));
#17482=CARTESIAN_POINT('Ctrl Pts',(-0.121921363946098,-0.034237873926493,
0.0615205540930479));
#17483=CARTESIAN_POINT('Ctrl Pts',(-0.110855003598394,-0.0736453296270277,
0.0641072127293806));
#17484=CARTESIAN_POINT('Ctrl Pts',(-0.0788915213442898,-0.107184815251071,
0.0666938713657133));
#17485=CARTESIAN_POINT('Ctrl Pts',(-0.0400617348236378,-0.120133683626334,
0.069280530002046));
#17486=CARTESIAN_POINT('Ctrl Pts',(-0.00123194830298627,-0.133082552001597,
0.0718671886383786));
#17487=CARTESIAN_POINT('Ctrl Pts',(0.0444641424842127,-0.125440803128081,
0.0744538472747112));
#17488=CARTESIAN_POINT('Ctrl Pts',(0.0769682295152699,-0.100563001286921,
0.0770405059110438));
#17489=CARTESIAN_POINT('Ctrl Pts',(0.109472316546327,-0.0756851994457607,
0.0796271645473764));
#17490=CARTESIAN_POINT('Ctrl Pts',(0.128784399821243,-0.0335713446369571,
0.0822138231837091));
#17491=CARTESIAN_POINT('Ctrl Pts',(0.126427276285523,0.00729262199647547,
0.0848004818200417));
#17492=CARTESIAN_POINT('Ctrl Pts',(0.124070152749803,0.0481565886299079,
0.0873871404563744));
#17493=CARTESIAN_POINT('Ctrl Pts',(0.100043822403448,0.0877706670879697,
0.0899737990927071));
#17494=CARTESIAN_POINT('Ctrl Pts',(0.0648947831756147,0.108746049780439,
0.0925604577290397));
#17495=CARTESIAN_POINT('Ctrl Pts',(0.0297457439477817,0.129721432472907,
0.0951471163653723));
#17496=CARTESIAN_POINT('Ctrl Pts',(-0.0165260041615291,0.132058119399784,
0.0977337750017049));
#17497=CARTESIAN_POINT('Ctrl Pts',(-0.0536093211433369,0.114730442741844,
0.100320433638038));
#17498=CARTESIAN_POINT('Ctrl Pts',(-0.0906926381251451,0.0974027660839045,
0.10290709227437));
#17499=CARTESIAN_POINT('Ctrl Pts',(-0.11858752397945,0.0604107258411485,
0.105493750910703));
#17500=CARTESIAN_POINT('Ctrl Pts',(-0.12504939731921,0.0199921027543164,
0.108080409547035));
#17501=CARTESIAN_POINT('Ctrl Pts',(-0.126099919499473,0.0134211506765118,
0.108500928818671));
#17502=CARTESIAN_POINT('Ctrl Pts',(-0.126583971845017,0.00675963476331471,
0.108921448090306));
#17503=CARTESIAN_POINT('Ctrl Pts',(-0.126529791093031,9.025049583615E-5,
0.109341967361942));
#17504=CARTESIAN_POINT('Origin',(0.,0.,0.12));
#17505=CARTESIAN_POINT('',(-0.126296536029262,-6.10717992316628E-5,0.159341967361942));
#17506=CARTESIAN_POINT('',(-0.126453631260982,-0.000102348163238207,0.145658032638058));
#17507=CARTESIAN_POINT('',(-0.12645,1.54856587752183E-17,0.12));
#17508=CARTESIAN_POINT('Ctrl Pts',(-0.126453631260982,-0.000102348163238207,
0.145658032638058));
#17509=CARTESIAN_POINT('Ctrl Pts',(-0.126183364177612,0.031552920325249,
0.143665210546026));
#17510=CARTESIAN_POINT('Ctrl Pts',(-0.114073771100105,0.0633928690595716,
0.141672388453994));
#17511=CARTESIAN_POINT('Ctrl Pts',(-0.0925489356314354,0.0864391430514358,
0.139679566361962));
#17512=CARTESIAN_POINT('Ctrl Pts',(-0.0646099631645552,0.116352924063146,
0.13709290772563));
#17513=CARTESIAN_POINT('Ctrl Pts',(-0.0208084524006029,0.131451366650306,
0.134506249089297));
#17514=CARTESIAN_POINT('Ctrl Pts',(0.0196287675426836,0.125106932552633,
0.131919590452964));
#17515=CARTESIAN_POINT('Ctrl Pts',(0.0600659874859703,0.11876249845496,
0.129332931816632));
#17516=CARTESIAN_POINT('Ctrl Pts',(0.097138916608591,0.0909751876724545,
0.126746273180299));
#17517=CARTESIAN_POINT('Ctrl Pts',(0.114574233156503,0.0539423598350403,
0.124159614543967));
#17518=CARTESIAN_POINT('Ctrl Pts',(0.132009549704415,0.0169095319976262,
0.121572955907634));
#17519=CARTESIAN_POINT('Ctrl Pts',(0.129807253677619,-0.0293688128946969,
0.118986297271301));
#17520=CARTESIAN_POINT('Ctrl Pts',(0.108934072954415,-0.0645786240759305,
0.116399638634969));
#17521=CARTESIAN_POINT('Ctrl Pts',(0.0880608922312115,-0.099788435257164,
0.113812979998636));
#17522=CARTESIAN_POINT('Ctrl Pts',(0.0485168268116012,-0.123929712727308,
0.111226321362303));
#17523=CARTESIAN_POINT('Ctrl Pts',(0.00765986125275547,-0.126405537442516,
0.108639662725971));
#17524=CARTESIAN_POINT('Ctrl Pts',(-0.0331971043060904,-0.128881362157723,
0.106053004089638));
#17525=CARTESIAN_POINT('Ctrl Pts',(-0.0753669700041717,-0.109691734117994,
0.103466345453305));
#17526=CARTESIAN_POINT('Ctrl Pts',(-0.100339039978837,-0.0772600332835736,
0.100879686816973));
#17527=CARTESIAN_POINT('Ctrl Pts',(-0.117142637704978,-0.0554368822612891,
0.0991391354240014));
#17528=CARTESIAN_POINT('Ctrl Pts',(-0.126159269908366,-0.0276178718881664,
0.0973985840310299));
#17529=CARTESIAN_POINT('Ctrl Pts',(-0.126349242904067,8.85860673823967E-5,
0.0956580326380584));
#17530=CARTESIAN_POINT('Ctrl Pts',(-0.126529791093031,9.025049583615E-5,
0.109341967361942));
#17531=CARTESIAN_POINT('Ctrl Pts',(-0.126250700293628,-0.0342644551610371,
0.111508106726639));
#17532=CARTESIAN_POINT('Ctrl Pts',(-0.111690189779818,-0.0688279388928191,
0.113674246091336));
#17533=CARTESIAN_POINT('Ctrl Pts',(-0.0867076257192948,-0.092297473337895,
0.115840385456033));
#17534=CARTESIAN_POINT('Ctrl Pts',(-0.0568751199544048,-0.120323220412367,
0.118427044092366));
#17535=CARTESIAN_POINT('Ctrl Pts',(-0.0121812475994092,-0.132529508630403,
0.121013702728699));
#17536=CARTESIAN_POINT('Ctrl Pts',(0.0277554439013372,-0.123558363290506,
0.123600361365031));
#17537=CARTESIAN_POINT('Ctrl Pts',(0.0676921354020838,-0.114587217950609,
0.126187020001364));
#17538=CARTESIAN_POINT('Ctrl Pts',(0.102871646048582,-0.0844386390527785,
0.128773678637697));
#17539=CARTESIAN_POINT('Ctrl Pts',(0.117851793294146,-0.0463464242807743,
0.131360337274029));
#17540=CARTESIAN_POINT('Ctrl Pts',(0.13283194053971,-0.00825420950877041,
0.133946995910362));
#17541=CARTESIAN_POINT('Ctrl Pts',(0.127612724384341,0.0377816411374068,
0.136533654546694));
#17542=CARTESIAN_POINT('Ctrl Pts',(0.104485135941302,0.0715534408109559,
0.139120313183027));
#17543=CARTESIAN_POINT('Ctrl Pts',(0.0813575474982633,0.105325240484505,
0.14170697181936));
#17544=CARTESIAN_POINT('Ctrl Pts',(0.0403215867675544,0.126832989185426,
0.144293630455692));
#17545=CARTESIAN_POINT('Ctrl Pts',(-0.000609841963000384,0.126635909896556,
0.146880289092025));
#17546=CARTESIAN_POINT('Ctrl Pts',(-0.0415412706935549,0.126438830607686,
0.149466947728358));
#17547=CARTESIAN_POINT('Ctrl Pts',(-0.0823681674239554,0.104536923329025,
0.15205360636469));
#17548=CARTESIAN_POINT('Ctrl Pts',(-0.10516942503222,0.0705438627883669,
0.154640265001023));
#17549=CARTESIAN_POINT('Ctrl Pts',(-0.118984510025511,0.0499477610899654,
0.156207499121329));
#17550=CARTESIAN_POINT('Ctrl Pts',(-0.126182304652747,0.0249129445447297,
0.157774733241635));
#17551=CARTESIAN_POINT('Ctrl Pts',(-0.126296536029262,-6.10717992316628E-5,
0.159341967361942));
#17552=CARTESIAN_POINT('Origin',(0.,0.,0.12));
#17553=CARTESIAN_POINT('',(-0.126625441102054,2.7778768752873E-5,0.209341967361942));
#17554=CARTESIAN_POINT('',(-0.126471935391749,0.000101176582396995,0.195658032638058));
#17555=CARTESIAN_POINT('',(-0.12645,1.54856587752183E-17,0.12));
#17556=CARTESIAN_POINT('',(0.0958116152722397,0.0825211298936481,0.24));
#17557=CARTESIAN_POINT('Ctrl Pts',(-0.126625441102054,2.7778768752873E-5,
0.209341967361942));
#17558=CARTESIAN_POINT('Ctrl Pts',(-0.126482885932031,-0.0388928622545336,
0.21180133566563));
#17559=CARTESIAN_POINT('Ctrl Pts',(-0.107125339127294,-0.077921419747323,
0.214260703969318));
#17560=CARTESIAN_POINT('Ctrl Pts',(-0.0759952538809665,-0.101287130411732,
0.216720072273006));
#17561=CARTESIAN_POINT('Ctrl Pts',(-0.0432539585932993,-0.12586218783339,
0.219306730909339));
#17562=CARTESIAN_POINT('Ctrl Pts',(0.0025100419330305,-0.133111106253138,
0.221893389545672));
#17563=CARTESIAN_POINT('Ctrl Pts',(0.0412155518054008,-0.119764891216682,
0.224480048182004));
#17564=CARTESIAN_POINT('Ctrl Pts',(0.0799210616777711,-0.106418676180227,
0.227066706818337));
#17565=CARTESIAN_POINT('Ctrl Pts',(0.111568080896182,-0.072477327687567,
0.229653365454669));
#17566=CARTESIAN_POINT('Ctrl Pts',(0.122246574267713,-0.0330282462555153,
0.232240024091002));
#17567=CARTESIAN_POINT('Ctrl Pts',(0.132925067639245,0.00642083517653631,
0.234826682727335));
#17568=CARTESIAN_POINT('Ctrl Pts',(0.122635035163896,0.0513776495479799,
0.237413341363667));
#17569=CARTESIAN_POINT('Ctrl Pts',(0.0958116152722397,0.0825211298936481,
0.24));
#17570=CARTESIAN_POINT('',(-0.0959791030802601,0.0826138105732953,0.24));
#17571=CARTESIAN_POINT('Origin',(0.,0.,0.24));
#17572=CARTESIAN_POINT('Ctrl Pts',(-0.0959791030802601,0.0826138105732953,
0.24));
#17573=CARTESIAN_POINT('Ctrl Pts',(-0.0710417758635208,0.111296717646776,
0.237599759089979));
#17574=CARTESIAN_POINT('Ctrl Pts',(-0.0322351762885183,0.128218895525122,
0.235199518179958));
#17575=CARTESIAN_POINT('Ctrl Pts',(0.00571352152256588,0.126497857083363,
0.232799277269937));
#17576=CARTESIAN_POINT('Ctrl Pts',(0.0466095526337785,0.124643152028446,
0.230212618633605));
#17577=CARTESIAN_POINT('Ctrl Pts',(0.0865092470399708,0.101136876245298,
0.227625959997272));
#17578=CARTESIAN_POINT('Ctrl Pts',(0.107920636628548,0.0662586835305903,
0.225039301360939));
#17579=CARTESIAN_POINT('Ctrl Pts',(0.129332026217125,0.0313804908158828,
0.222452642724607));
#17580=CARTESIAN_POINT('Ctrl Pts',(0.132255110988087,-0.014869618830384,
0.219865984088274));
#17581=CARTESIAN_POINT('Ctrl Pts',(0.115395215428634,-0.0521699181865619,
0.217279325451942));
#17582=CARTESIAN_POINT('Ctrl Pts',(0.0985353198691812,-0.0894702175427398,
0.214692666815609));
#17583=CARTESIAN_POINT('Ctrl Pts',(0.0618924439793129,-0.117820706608829,
0.212106008179276));
#17584=CARTESIAN_POINT('Ctrl Pts',(0.0215571925812854,-0.12478734248304,
0.209519349542944));
#17585=CARTESIAN_POINT('Ctrl Pts',(-0.0187780588167422,-0.13175397835725,
0.206932690906611));
#17586=CARTESIAN_POINT('Ctrl Pts',(-0.0628056857229291,-0.117336761039583,
0.204346032270278));
#17587=CARTESIAN_POINT('Ctrl Pts',(-0.0912027768750998,-0.0878586653637446,
0.201759373633946));
#17588=CARTESIAN_POINT('Ctrl Pts',(-0.113530209130371,-0.0646812849521466,
0.199725593301983));
#17589=CARTESIAN_POINT('Ctrl Pts',(-0.126194825294183,-0.0321932513395888,
0.197691812970021));
#17590=CARTESIAN_POINT('Ctrl Pts',(-0.126471935391749,0.000101176582396995,
0.195658032638058));
#17591=CARTESIAN_POINT('Origin',(0.,0.,0.350421172358873));
#17592=CARTESIAN_POINT('',(-0.154453350152392,-8.79343647196378E-5,0.0295788276411275));
#17593=CARTESIAN_POINT('',(-0.15422847552802,0.000108763211052777,0.025421172358873));
#17594=CARTESIAN_POINT('',(-0.1543,-1.01731279388251E-15,0.350421172358873));
#17595=CARTESIAN_POINT('',(0.15408394018464,-0.00816268198427004,0.));
#17596=CARTESIAN_POINT('Ctrl Pts',(-0.15422847552802,0.000108763211052763,
0.025421172358873));
#17597=CARTESIAN_POINT('Ctrl Pts',(-0.154338737393477,0.0139570514561378,
0.0247074241482466));
#17598=CARTESIAN_POINT('Ctrl Pts',(-0.146387882101843,0.0778735560251454,
0.0214070173012875));
#17599=CARTESIAN_POINT('Ctrl Pts',(-0.0581466660421577,0.171532975008042,
0.0155199518179959));
#17600=CARTESIAN_POINT('Ctrl Pts',(0.109502662757235,0.144085240745689,
0.00775997590899784));
#17601=CARTESIAN_POINT('Ctrl Pts',(0.156737212705124,0.0419221657566679,
0.00258665863633264));
#17602=CARTESIAN_POINT('Ctrl Pts',(0.15408394018464,-0.00816268198427004,
0.));
#17603=CARTESIAN_POINT('',(0.129620323775263,-0.0841289546921688,3.62607491890453E-17));
#17604=CARTESIAN_POINT('Origin',(0.,0.,0.));
#17605=CARTESIAN_POINT('Ctrl Pts',(-0.154453350152392,-8.7934364719636E-5,
0.0295788276411275));
#17606=CARTESIAN_POINT('Ctrl Pts',(-0.154150470777978,0.0441115087317509,
0.0272927766101045));
#17607=CARTESIAN_POINT('Ctrl Pts',(-0.111454882743928,0.138841433785012,
0.0224200669427489));
#17608=CARTESIAN_POINT('Ctrl Pts',(0.0476444145610997,0.174632482457551,
0.0149606986390605));
#17609=CARTESIAN_POINT('Ctrl Pts',(0.168251138196633,0.0613688951001999,
0.0073871404563744));
#17610=CARTESIAN_POINT('Ctrl Pts',(0.154676764047789,-0.0451013867871701,
0.00240024091002087));
#17611=CARTESIAN_POINT('Ctrl Pts',(0.129620323775263,-0.0841289546921688,
1.57209315010398E-17));
#17612=CARTESIAN_POINT('Origin',(0.,0.,0.350421172358873));
#17613=CARTESIAN_POINT('',(-0.154177051641736,0.000108096719625833,0.0795788276411275));
#17614=CARTESIAN_POINT('',(-0.154234284709463,-0.000121519309271207,0.075421172358873));
#17615=CARTESIAN_POINT('',(-0.1543,-1.01731279388251E-15,0.350421172358873));
#17616=CARTESIAN_POINT('Ctrl Pts',(-0.154234284709463,-0.000121519309271208,
0.0754211723588731));
#17617=CARTESIAN_POINT('Ctrl Pts',(-0.153947235272697,0.0359820467524117,
0.0735607092995758));
#17618=CARTESIAN_POINT('Ctrl Pts',(-0.123557126730793,0.122717061869437,
0.0691135876039459));
#17619=CARTESIAN_POINT('Ctrl Pts',(0.0191012565771036,0.180005302104073,
0.0620798072719832));
#17620=CARTESIAN_POINT('Ctrl Pts',(0.159724738700703,0.0851738948996701,
0.0543198313629854));
#17621=CARTESIAN_POINT('Ctrl Pts',(0.160113920417758,-0.0844204212478698,
0.0465598554539874));
#17622=CARTESIAN_POINT('Ctrl Pts',(0.0199582426985643,-0.179924098035372,
0.0387998795449896));
#17623=CARTESIAN_POINT('Ctrl Pts',(-0.123251388539896,-0.123176028715441,
0.0317536518466181));
#17624=CARTESIAN_POINT('Ctrl Pts',(-0.153939142967466,-0.0362298265692857,
0.0272940827845792));
#17625=CARTESIAN_POINT('Ctrl Pts',(-0.15422847552802,0.000108763211052763,
0.025421172358873));
#17626=CARTESIAN_POINT('Ctrl Pts',(-0.154177051641736,0.000108096719625859,
0.0795788276411275));
#17627=CARTESIAN_POINT('Ctrl Pts',(-0.154289739603949,0.0165429814548096,
0.0787327203977663));
#17628=CARTESIAN_POINT('Ctrl Pts',(-0.144420757340354,0.0830897487115299,
0.0752999545180725));
#17629=CARTESIAN_POINT('Ctrl Pts',(-0.0494457976037486,0.174130301808973,
0.0692805300020459));
#17630=CARTESIAN_POINT('Ctrl Pts',(0.11640175885633,0.13862511662766,0.061520554093048));
#17631=CARTESIAN_POINT('Ctrl Pts',(0.18005704388064,-0.0185795878987759,
0.0537605781840501));
#17632=CARTESIAN_POINT('Ctrl Pts',(0.0856431484406112,-0.159474177462153,
0.0460006022750521));
#17633=CARTESIAN_POINT('Ctrl Pts',(-0.0839657292871194,-0.160363143120653,
0.0382406263660544));
#17634=CARTESIAN_POINT('Ctrl Pts',(-0.151599316432495,-0.0616831513139142,
0.0327667014880793));
#17635=CARTESIAN_POINT('Ctrl Pts',(-0.154493177716258,-0.00590000442131094,
0.0298794352464371));
#17636=CARTESIAN_POINT('Ctrl Pts',(-0.154453350152392,-8.7934364719636E-5,
0.0295788276411275));
#17637=CARTESIAN_POINT('Origin',(0.,0.,0.350421172358873));
#17638=CARTESIAN_POINT('',(-0.154304431028624,-0.000124889850439479,0.129578827641127));
#17639=CARTESIAN_POINT('',(-0.154397364694779,0.000110127730384366,0.125421172358873));
#17640=CARTESIAN_POINT('',(-0.1543,-1.01731279388251E-15,0.350421172358873));
#17641=CARTESIAN_POINT('Ctrl Pts',(-0.154397364694779,0.000110127730384357,
0.125421172358873));
#17642=CARTESIAN_POINT('Ctrl Pts',(-0.154463478494948,0.00824841157753406,
0.125000653087238));
#17643=CARTESIAN_POINT('Ctrl Pts',(-0.150239588102603,0.0663774823757793,
0.121993475179269));
#17644=CARTESIAN_POINT('Ctrl Pts',(-0.0766286530280003,0.163994611436961,
0.116399638634969));
#17645=CARTESIAN_POINT('Ctrl Pts',(0.0927599764682439,0.155440618724813,
0.108639662725971));
#17646=CARTESIAN_POINT('Ctrl Pts',(0.180714016146597,0.0104239566588842,
0.100879686816973));
#17647=CARTESIAN_POINT('Ctrl Pts',(0.11001758793024,-0.143743725357685,
0.093119710907975));
#17648=CARTESIAN_POINT('Ctrl Pts',(-0.0572637123892103,-0.171718146500831,
0.0853597349989769));
#17649=CARTESIAN_POINT('Ctrl Pts',(-0.146220320052713,-0.0783754111826042,
0.0794602221492764));
#17650=CARTESIAN_POINT('Ctrl Pts',(-0.154346328875204,-0.0142138442593302,
0.0761473679359084));
#17651=CARTESIAN_POINT('Ctrl Pts',(-0.154234284709463,-0.000121519309271208,
0.0754211723588731));
#17652=CARTESIAN_POINT('Ctrl Pts',(-0.154304431028624,-0.000124889850439474,
0.129578827641127));
#17653=CARTESIAN_POINT('Ctrl Pts',(-0.153974638929265,0.0385022981904757,
0.127586005549095));
#17654=CARTESIAN_POINT('Ctrl Pts',(-0.120018027207353,0.127784966030512,
0.123006524820731));
#17655=CARTESIAN_POINT('Ctrl Pts',(0.0280571680938306,0.178826694862324,
0.115840385456033));
#17656=CARTESIAN_POINT('Ctrl Pts',(0.163771354656592,0.0771047007047774,
0.108080409547035));
#17657=CARTESIAN_POINT('Ctrl Pts',(0.155709331479018,-0.0923080778690166,
0.100320433638038));
#17658=CARTESIAN_POINT('Ctrl Pts',(0.0109489686262093,-0.180682908560435,
0.0925604577290397));
#17659=CARTESIAN_POINT('Ctrl Pts',(-0.126591758993125,-0.118094248159534,
0.0856465890634029));
#17660=CARTESIAN_POINT('Ctrl Pts',(-0.153945238013925,-0.0337005743957639,
0.0813193790340989));
#17661=CARTESIAN_POINT('Ctrl Pts',(-0.154177051641736,0.000108096719625859,
0.0795788276411275));
#17662=CARTESIAN_POINT('Origin',(0.,0.,0.350421172358873));
#17663=CARTESIAN_POINT('',(-0.154326766555531,0.000123460234585843,0.179578827641127));
#17664=CARTESIAN_POINT('',(-0.154112736333057,-7.45225671948511E-5,0.175421172358873));
#17665=CARTESIAN_POINT('',(-0.1543,-1.01731279388251E-15,0.350421172358873));
#17666=CARTESIAN_POINT('Ctrl Pts',(-0.154112736333057,-7.45225671948471E-5,
0.175421172358873));
#17667=CARTESIAN_POINT('Ctrl Pts',(-0.153973346049181,0.0303998999070902,
0.173853938238567));
#17668=CARTESIAN_POINT('Ctrl Pts',(-0.130694151755309,0.111367805862998,
0.169700045481928));
#17669=CARTESIAN_POINT('Ctrl Pts',(-0.000871711368246156,0.181012066871201,
0.162959494088956));
#17670=CARTESIAN_POINT('Ctrl Pts',(0.149350085565286,0.102277888352765,
0.155199518179958));
#17671=CARTESIAN_POINT('Ctrl Pts',(0.168456255263351,-0.0662471829332422,
0.14743954227096));
#17672=CARTESIAN_POINT('Ctrl Pts',(0.0396733728729688,-0.17661315503135,
0.139679566361963));
#17673=CARTESIAN_POINT('Ctrl Pts',(-0.115072782317819,-0.134350623919955,
0.1323401097246));
#17674=CARTESIAN_POINT('Ctrl Pts',(-0.154056805498669,-0.041811035439686,
0.12758731172357));
#17675=CARTESIAN_POINT('Ctrl Pts',(-0.154397364694779,0.000110127730384357,
0.125421172358873));
#17676=CARTESIAN_POINT('Ctrl Pts',(-0.154326766555531,0.000123460234585825,
0.179578827641127));
#17677=CARTESIAN_POINT('Ctrl Pts',(-0.154418689716183,0.0108361910665024,
0.179025949336757));
#17678=CARTESIAN_POINT('Ctrl Pts',(-0.148597337680631,0.071569631208062,
0.175886412396054));
#17679=CARTESIAN_POINT('Ctrl Pts',(-0.0683530255288039,0.167611467503216,
0.170160216819019));
#17680=CARTESIAN_POINT('Ctrl Pts',(0.100397202365132,0.150621028353064,
0.162400240910021));
#17681=CARTESIAN_POINT('Ctrl Pts',(0.18100910679194,0.00139719974911195,
0.154640265001023));
#17682=CARTESIAN_POINT('Ctrl Pts',(0.102711092909207,-0.149052183789333,
0.146880289092025));
#17683=CARTESIAN_POINT('Ctrl Pts',(-0.0657574679958034,-0.168648048308422,
0.139120313183027));
#17684=CARTESIAN_POINT('Ctrl Pts',(-0.148058381688037,-0.0731761882111772,
0.133353159366061));
#17685=CARTESIAN_POINT('Ctrl Pts',(-0.154402705029802,-0.0116353181791797,
0.130172664185428));
#17686=CARTESIAN_POINT('Ctrl Pts',(-0.154304431028624,-0.000124889850439474,
0.129578827641127));
#17687=CARTESIAN_POINT('Origin',(0.,0.,0.350421172358873));
#17688=CARTESIAN_POINT('',(-0.154128406284035,-0.000157308197905263,0.229578827641128));
#17689=CARTESIAN_POINT('',(-0.154514081154978,3.38969080117728E-5,0.225421172358873));
#17690=CARTESIAN_POINT('',(-0.1543,-1.01731279388251E-15,0.350421172358873));
#17691=CARTESIAN_POINT('',(-0.0398513841857245,-0.149064942821851,0.24));
#17692=CARTESIAN_POINT('Ctrl Pts',(-0.0398513841857245,-0.149064942821851,
0.24));
#17693=CARTESIAN_POINT('Ctrl Pts',(-0.0883048112969314,-0.136111285829332,
0.237413341363667));
#17694=CARTESIAN_POINT('Ctrl Pts',(-0.143745772087175,-0.0847488633265083,
0.233939617244043));
#17695=CARTESIAN_POINT('Ctrl Pts',(-0.154234229255939,-0.017399338864059,
0.230465893124419));
#17696=CARTESIAN_POINT('Ctrl Pts',(-0.154128406284035,-0.00015730819790527,
0.229578827641128));
#17697=CARTESIAN_POINT('',(0.0399565498027962,-0.149273502906638,0.24));
#17698=CARTESIAN_POINT('Origin',(0.,0.,0.24));
#17699=CARTESIAN_POINT('Ctrl Pts',(0.0399565498027963,-0.149273502906638,
0.24));
#17700=CARTESIAN_POINT('Ctrl Pts',(-0.00490373130458673,-0.161043406468747,
0.237599759089979));
#17701=CARTESIAN_POINT('Ctrl Pts',(-0.107666111297752,-0.141562671532916,
0.23274014987627));
#17702=CARTESIAN_POINT('Ctrl Pts',(-0.154340128899266,-0.0474588267763927,
0.227880540662561));
#17703=CARTESIAN_POINT('Ctrl Pts',(-0.154514081154978,3.3896908011755E-5,
0.225421172358873));
#17704=CARTESIAN_POINT('Origin',(0.,0.,0.350421172358873));
#17705=CARTESIAN_POINT('Ctrl Pts',(-0.154514081154978,3.3896908011755E-5,
0.225421172358873));
#17706=CARTESIAN_POINT('Ctrl Pts',(-0.154523084458981,0.00249199339844659,
0.225293882026228));
#17707=CARTESIAN_POINT('Ctrl Pts',(-0.153375868586475,0.0548933889046004,
0.222579933057251));
#17708=CARTESIAN_POINT('Ctrl Pts',(-0.0942515706791253,0.154556313135293,
0.217279325451942));
#17709=CARTESIAN_POINT('Ctrl Pts',(0.0750450248431312,0.164716481511431,
0.209519349542944));
#17710=CARTESIAN_POINT('Ctrl Pts',(0.178461260043253,0.0303012077178856,
0.201759373633945));
#17711=CARTESIAN_POINT('Ctrl Pts',(0.125203781387627,-0.130731709675357,
0.193999397724948));
#17712=CARTESIAN_POINT('Ctrl Pts',(-0.0379704533096903,-0.17698585337688,
0.18623942181595));
#17713=CARTESIAN_POINT('Ctrl Pts',(-0.141587477595567,-0.0899051669249145,
0.180046680027258));
#17714=CARTESIAN_POINT('Ctrl Pts',(-0.154203404262525,-0.019896942829432,
0.176440596874899));
#17715=CARTESIAN_POINT('Ctrl Pts',(-0.154112736333057,-7.45225671948471E-5,
0.175421172358873));
#17716=CARTESIAN_POINT('Ctrl Pts',(-0.154128406284035,-0.00015730819790527,
0.229578827641128));
#17717=CARTESIAN_POINT('Ctrl Pts',(-0.153925652370292,0.0328779499839183,
0.227879234488086));
#17718=CARTESIAN_POINT('Ctrl Pts',(-0.127638532780061,0.116591914860373,
0.223592982698713));
#17719=CARTESIAN_POINT('Ctrl Pts',(0.00818767200092134,0.180778621679153,
0.216720072273006));
#17720=CARTESIAN_POINT('Ctrl Pts',(0.154249898498561,0.0947283641859207,
0.208960096364008));
#17721=CARTESIAN_POINT('Ctrl Pts',(0.164950538597243,-0.0745810526211722,
0.201200120455011));
#17722=CARTESIAN_POINT('Ctrl Pts',(0.0308106631569891,-0.178364693496558,
0.193440144546012));
#17723=CARTESIAN_POINT('Ctrl Pts',(-0.118879635670858,-0.129347344159377,
0.186233046941385));
#17724=CARTESIAN_POINT('Ctrl Pts',(-0.153988624301243,-0.0392836590090855,
0.18161260797309));
#17725=CARTESIAN_POINT('Ctrl Pts',(-0.154326766555531,0.000123460234585825,
0.179578827641127));
#17726=CARTESIAN_POINT('Ctrl Pts',(0.0958116152722397,0.0825211298936481,
0.24));
#17727=CARTESIAN_POINT('Ctrl Pts',(0.122635035163896,0.0513776495479799,
0.237413341363667));
#17728=CARTESIAN_POINT('Ctrl Pts',(0.143215100114593,-0.0385359791949074,
0.232240024091002));
#17729=CARTESIAN_POINT('Ctrl Pts',(0.0482740424593604,-0.140360024672886,
0.224480048182004));
#17730=CARTESIAN_POINT('Ctrl Pts',(-0.0890179591196291,-0.118613269413641,
0.216720072273006));
#17731=CARTESIAN_POINT('Ctrl Pts',(-0.148173729266643,0.00709031985706173,
0.208960096364008));
#17732=CARTESIAN_POINT('Ctrl Pts',(-0.0772398646297824,0.126660050524678,
0.20120012045501));
#17733=CARTESIAN_POINT('Ctrl Pts',(0.0614999571705377,0.134986384232796,
0.193440144546013));
#17734=CARTESIAN_POINT('Ctrl Pts',(0.146250332679645,0.0248320655601208,
0.185680168637014));
#17735=CARTESIAN_POINT('Ctrl Pts',(0.102605431992647,-0.107135610424167,
0.177920192728017));
#17736=CARTESIAN_POINT('Ctrl Pts',(-0.0311170694815965,-0.145041225920327,
0.170160216819019));
#17737=CARTESIAN_POINT('Ctrl Pts',(-0.137521919612742,-0.0556176253575994,
0.162400240910021));
#17738=CARTESIAN_POINT('Ctrl Pts',(-0.123195064154356,0.0826350160503635,
0.154640265001023));
#17739=CARTESIAN_POINT('Ctrl Pts',(-0.000714373963154436,0.148340737886347,
0.146880289092025));
#17740=CARTESIAN_POINT('Ctrl Pts',(0.122393508228972,0.0838174917835845,
0.139120313183027));
#17741=CARTESIAN_POINT('Ctrl Pts',(0.138051156695079,-0.0542900601549481,
0.131360337274029));
#17742=CARTESIAN_POINT('Ctrl Pts',(0.032512624755586,-0.14473579684844,
0.123600361365031));
#17743=CARTESIAN_POINT('Ctrl Pts',(-0.101568992309399,-0.108116932194331,
0.115840385456033));
#17744=CARTESIAN_POINT('Ctrl Pts',(-0.146482409833755,0.0234186855983926,
0.108080409547036));
#17745=CARTESIAN_POINT('Ctrl Pts',(-0.0627977522708403,0.13439480632666,
0.100320433638038));
#17746=CARTESIAN_POINT('Ctrl Pts',(0.076017492057093,0.127384745546031,
0.0925604577290397));
#17747=CARTESIAN_POINT('Ctrl Pts',(0.148096483096158,0.00854251017184644,
0.0848004818200417));
#17748=CARTESIAN_POINT('Ctrl Pts',(0.0901602332714121,-0.117799054254564,
0.0770405059110438));
#17749=CARTESIAN_POINT('Ctrl Pts',(-0.0469280390901857,-0.140724300875114,
0.069280530002046));
#17750=CARTESIAN_POINT('Ctrl Pts',(-0.142818485852497,-0.0401058440029853,
0.0615205540930479));
#17751=CARTESIAN_POINT('Ctrl Pts',(-0.113326201176411,0.0957204333280909,
0.0537605781840501));
#17752=CARTESIAN_POINT('Ctrl Pts',(0.0156536221268617,0.147515686656254,
0.0460006022750521));
#17753=CARTESIAN_POINT('Ctrl Pts',(0.130895613795878,0.0698006416724775,
0.0382406263660543));
#17754=CARTESIAN_POINT('Ctrl Pts',(0.13121455111358,-0.0691831643991777,
0.0304806504570563));
#17755=CARTESIAN_POINT('Ctrl Pts',(0.0163559286405278,-0.147449139316739,
0.0227206745480584));
#17756=CARTESIAN_POINT('Ctrl Pts',(-0.112893560070904,-0.0962328986104914,
0.0149606986390606));
#17757=CARTESIAN_POINT('Ctrl Pts',(-0.142972035491037,0.0393992613429074,
0.00720072273006258));
#17758=CARTESIAN_POINT('Ctrl Pts',(-0.0476516261894416,0.140572551456688,
-0.000559253178935252));
#17759=CARTESIAN_POINT('Ctrl Pts',(0.0897382482543901,0.118078928660352,
-0.00831922908793326));
#17760=CARTESIAN_POINT('Ctrl Pts',(0.128447313976429,0.0343555272840613,
-0.0134925463605985));
#17761=CARTESIAN_POINT('Ctrl Pts',(0.126272937371016,-0.00668937872268922,
-0.0160792049969311));
#17762=CARTESIAN_POINT('Ctrl Pts',(0.102845629995666,0.0885794229410663,
0.245359734998977));
#17763=CARTESIAN_POINT('Ctrl Pts',(0.13163829265517,0.0551495423644061,
0.242773076362644));
#17764=CARTESIAN_POINT('Ctrl Pts',(0.153729244145676,-0.0413651001137901,
0.237599759089979));
#17765=CARTESIAN_POINT('Ctrl Pts',(0.0518180837997932,-0.150664563191773,
0.229839783180981));
#17766=CARTESIAN_POINT('Ctrl Pts',(-0.0955532172229155,-0.127321268762976,
0.222079807271983));
#17767=CARTESIAN_POINT('Ctrl Pts',(-0.159051911315084,0.00761085605850937,
0.214319831362985));
#17768=CARTESIAN_POINT('Ctrl Pts',(-0.0829104333128967,0.135958804728216,
0.206559855453988));
#17769=CARTESIAN_POINT('Ctrl Pts',(0.0660149797280689,0.144896416659008,
0.19879987954499));
#17770=CARTESIAN_POINT('Ctrl Pts',(0.156987308467515,0.0266551129460425,
0.191039903635992));
#17771=CARTESIAN_POINT('Ctrl Pts',(0.110138215124307,-0.11500097684123,
0.183279927726994));
#17772=CARTESIAN_POINT('Ctrl Pts',(-0.0334015307576278,-0.155689435072511,
0.175519951817996));
#17773=CARTESIAN_POINT('Ctrl Pts',(-0.147618098500879,-0.0597007962188336,
0.167759975908998));
#17774=CARTESIAN_POINT('Ctrl Pts',(-0.13223943620312,0.0887016700559064,
0.16));
#17775=CARTESIAN_POINT('Ctrl Pts',(-0.000766819764851659,0.159231180881298,
0.152240024091002));
#17776=CARTESIAN_POINT('Ctrl Pts',(0.131379034007743,0.0899709573066447,
0.144480048182004));
#17777=CARTESIAN_POINT('Ctrl Pts',(0.14818618955117,-0.0582757677477129,
0.136720072273006));
#17778=CARTESIAN_POINT('Ctrl Pts',(0.0348995407947136,-0.15536158290941,
0.128960096364009));
#17779=CARTESIAN_POINT('Ctrl Pts',(-0.109025685167754,-0.116054342400242,
0.12120012045501));
#17780=CARTESIAN_POINT('Ctrl Pts',(-0.157236423577976,0.0251379696208395,
0.113440144546013));
#17781=CARTESIAN_POINT('Ctrl Pts',(-0.0674080525232269,0.144261408030094,
0.105680168637014));
#17782=CARTESIAN_POINT('Ctrl Pts',(0.0815983201941432,0.136736703272292,
0.0979201927280168));
#17783=CARTESIAN_POINT('Ctrl Pts',(0.158968994112971,0.00916965900085902,
0.0901602168190187));
#17784=CARTESIAN_POINT('Ctrl Pts',(0.0967793514910216,-0.126447277955604,
0.0824002409100209));
#17785=CARTESIAN_POINT('Ctrl Pts',(-0.0503732635231939,-0.151055582750353,
0.0746402650010229));
#17786=CARTESIAN_POINT('Ctrl Pts',(-0.15330351242688,-0.0430502166284845,
0.066880289092025));
#17787=CARTESIAN_POINT('Ctrl Pts',(-0.121646050135849,0.102747753924341,
0.0591203131830272));
#17788=CARTESIAN_POINT('Ctrl Pts',(0.0168028336102756,0.158345558472194,
0.0513603372740292));
#17789=CARTESIAN_POINT('Ctrl Pts',(0.140505322097486,0.074925059414875,
0.0436003613650313));
#17790=CARTESIAN_POINT('Ctrl Pts',(0.140847674214973,-0.0742622500154084,
0.0358403854560334));
#17791=CARTESIAN_POINT('Ctrl Pts',(0.0175566999932067,-0.158274125556283,
0.0280804095470355));
#17792=CARTESIAN_POINT('Ctrl Pts',(-0.121181646661057,-0.103297841872129,
0.0203204336380376));
#17793=CARTESIAN_POINT('Ctrl Pts',(-0.153468334920127,0.0422917601656304,
0.0125604577290396));
#17794=CARTESIAN_POINT('Ctrl Pts',(-0.0511499728070136,0.150892692640473,
0.00480048182004178));
#17795=CARTESIAN_POINT('Ctrl Pts',(0.0963263864220051,0.126747699355464,
-0.00295949408895622));
#17796=CARTESIAN_POINT('Ctrl Pts',(0.137877280219327,0.0368777401082635,
-0.00813281136162143));
#17797=CARTESIAN_POINT('Ctrl Pts',(0.135543271642224,-0.00718047980988283,
-0.0107194699979541));
#17798=CARTESIAN_POINT('Ctrl Pts',(0.109879644719093,0.0946377159884845,
0.250719469997954));
#17799=CARTESIAN_POINT('Ctrl Pts',(0.140641550146443,0.0589214351808321,
0.248132811361621));
#17800=CARTESIAN_POINT('Ctrl Pts',(0.164243388176759,-0.0441942210326729,
0.242959494088956));
#17801=CARTESIAN_POINT('Ctrl Pts',(0.055362125140226,-0.160969101710661,
0.235199518179958));
#17802=CARTESIAN_POINT('Ctrl Pts',(-0.102088475326202,-0.13602926811231,
0.227439542270961));
#17803=CARTESIAN_POINT('Ctrl Pts',(-0.169930093363525,0.00813139225995705,
0.219679566361962));
#17804=CARTESIAN_POINT('Ctrl Pts',(-0.0885810019960112,0.145257558931755,
0.211919590452965));
#17805=CARTESIAN_POINT('Ctrl Pts',(0.0705300022856002,0.154806449085219,
0.204159614543967));
#17806=CARTESIAN_POINT('Ctrl Pts',(0.167724284255384,0.0284781603319641,
0.196399638634969));
#17807=CARTESIAN_POINT('Ctrl Pts',(0.117670998255967,-0.122866343258294,
0.188639662725971));
#17808=CARTESIAN_POINT('Ctrl Pts',(-0.0356859920336591,-0.166337644224695,
0.180879686816973));
#17809=CARTESIAN_POINT('Ctrl Pts',(-0.157714277389017,-0.0637839670800676,
0.173119710907975));
#17810=CARTESIAN_POINT('Ctrl Pts',(-0.141283808251885,0.0947683240614489,
0.165359734998977));
#17811=CARTESIAN_POINT('Ctrl Pts',(-0.000819265566548849,0.17012162387625,
0.157599759089979));
#17812=CARTESIAN_POINT('Ctrl Pts',(0.140364559786514,0.0961244228297045,
0.149839783180981));
#17813=CARTESIAN_POINT('Ctrl Pts',(0.158321222407261,-0.0622614753404775,
0.142079807271983));
#17814=CARTESIAN_POINT('Ctrl Pts',(0.0372864568338413,-0.16598736897038,
0.134319831362986));
#17815=CARTESIAN_POINT('Ctrl Pts',(-0.116482378026109,-0.123991752606152,
0.126559855453987));
#17816=CARTESIAN_POINT('Ctrl Pts',(-0.167990437322196,0.0268572536432864,
0.11879987954499));
#17817=CARTESIAN_POINT('Ctrl Pts',(-0.0720183527756138,0.154128009733527,
0.111039903635992));
#17818=CARTESIAN_POINT('Ctrl Pts',(0.0871791483311938,0.146088660998552,
0.103279927726994));
#17819=CARTESIAN_POINT('Ctrl Pts',(0.169841505129784,0.00979680782987164,
0.0955199518179957));
#17820=CARTESIAN_POINT('Ctrl Pts',(0.103398469710631,-0.135095501656644,
0.0877599759089979));
#17821=CARTESIAN_POINT('Ctrl Pts',(-0.0538184879562023,-0.161386864625592,
0.08));
#17822=CARTESIAN_POINT('Ctrl Pts',(-0.163788539001263,-0.0459945892539838,
0.0722400240910021));
#17823=CARTESIAN_POINT('Ctrl Pts',(-0.129965899095288,0.10977507452059,
0.0644800481820042));
#17824=CARTESIAN_POINT('Ctrl Pts',(0.0179520450936897,0.169175430288133,
0.0567200722730062));
#17825=CARTESIAN_POINT('Ctrl Pts',(0.150115030399095,0.0800494771572726,
0.0489600963640084));
#17826=CARTESIAN_POINT('Ctrl Pts',(0.150480797316365,-0.0793413356316391,
0.0412001204550104));
#17827=CARTESIAN_POINT('Ctrl Pts',(0.0187574713458855,-0.169099111795828,
0.0334401445460125));
#17828=CARTESIAN_POINT('Ctrl Pts',(-0.129469733251211,-0.110362785133767,
0.0256801686370146));
#17829=CARTESIAN_POINT('Ctrl Pts',(-0.163964634349217,0.0451842589883535,
0.0179201927280167));
#17830=CARTESIAN_POINT('Ctrl Pts',(-0.0546483194245858,0.161212833824257,
0.0101602168190188));
#17831=CARTESIAN_POINT('Ctrl Pts',(0.10291452458962,0.135416470050577,0.00240024091002082));
#17832=CARTESIAN_POINT('Ctrl Pts',(0.147307246462226,0.0393999529324658,
-0.00277307636264439));
#17833=CARTESIAN_POINT('Ctrl Pts',(0.144813605913432,-0.00767158089707644,
-0.00535973499897704));
#17834=CARTESIAN_POINT('Ctrl Pts',(0.116913659442519,0.100696009035903,
0.256079204996931));
#17835=CARTESIAN_POINT('Ctrl Pts',(0.149644807637716,0.0626933279972582,
0.253492546360598));
#17836=CARTESIAN_POINT('Ctrl Pts',(0.174757532207842,-0.0470233419515556,
0.248319229087933));
#17837=CARTESIAN_POINT('Ctrl Pts',(0.0589061664806588,-0.171273640229548,
0.240559253178935));
#17838=CARTESIAN_POINT('Ctrl Pts',(-0.108623733429488,-0.144737267461644,
0.232799277269938));
#17839=CARTESIAN_POINT('Ctrl Pts',(-0.180808275411966,0.00865192846140473,
0.225039301360939));
#17840=CARTESIAN_POINT('Ctrl Pts',(-0.0942515706791253,0.154556313135293,
0.217279325451942));
#17841=CARTESIAN_POINT('Ctrl Pts',(0.0750450248431312,0.164716481511431,
0.209519349542944));
#17842=CARTESIAN_POINT('Ctrl Pts',(0.178461260043253,0.0303012077178856,
0.201759373633945));
#17843=CARTESIAN_POINT('Ctrl Pts',(0.125203781387627,-0.130731709675357,
0.193999397724948));
#17844=CARTESIAN_POINT('Ctrl Pts',(-0.0379704533096903,-0.17698585337688,
0.18623942181595));
#17845=CARTESIAN_POINT('Ctrl Pts',(-0.167810456277154,-0.0678671379413016,
0.178479445906952));
#17846=CARTESIAN_POINT('Ctrl Pts',(-0.150328180300649,0.100834978066992,
0.170719469997954));
#17847=CARTESIAN_POINT('Ctrl Pts',(-0.000871711368246156,0.181012066871201,
0.162959494088956));
#17848=CARTESIAN_POINT('Ctrl Pts',(0.149350085565286,0.102277888352765,
0.155199518179958));
#17849=CARTESIAN_POINT('Ctrl Pts',(0.168456255263351,-0.0662471829332422,
0.14743954227096));
#17850=CARTESIAN_POINT('Ctrl Pts',(0.0396733728729688,-0.17661315503135,
0.139679566361963));
#17851=CARTESIAN_POINT('Ctrl Pts',(-0.123939070884463,-0.131929162812062,
0.131919590452964));
#17852=CARTESIAN_POINT('Ctrl Pts',(-0.178744451066417,0.0285765376657333,
0.124159614543967));
#17853=CARTESIAN_POINT('Ctrl Pts',(-0.0766286530280003,0.163994611436961,
0.116399638634969));
#17854=CARTESIAN_POINT('Ctrl Pts',(0.0927599764682439,0.155440618724813,
0.108639662725971));
#17855=CARTESIAN_POINT('Ctrl Pts',(0.180714016146597,0.0104239566588842,
0.100879686816973));
#17856=CARTESIAN_POINT('Ctrl Pts',(0.11001758793024,-0.143743725357685,
0.093119710907975));
#17857=CARTESIAN_POINT('Ctrl Pts',(-0.0572637123892103,-0.171718146500831,
0.0853597349989769));
#17858=CARTESIAN_POINT('Ctrl Pts',(-0.174273565575645,-0.048938961879483,
0.0775997590899791));
#17859=CARTESIAN_POINT('Ctrl Pts',(-0.138285748054726,0.11680239511684,
0.0698397831809812));
#17860=CARTESIAN_POINT('Ctrl Pts',(0.0191012565771036,0.180005302104073,
0.0620798072719832));
#17861=CARTESIAN_POINT('Ctrl Pts',(0.159724738700703,0.0851738948996701,
0.0543198313629854));
#17862=CARTESIAN_POINT('Ctrl Pts',(0.160113920417758,-0.0844204212478698,
0.0465598554539874));
#17863=CARTESIAN_POINT('Ctrl Pts',(0.0199582426985643,-0.179924098035372,
0.0387998795449896));
#17864=CARTESIAN_POINT('Ctrl Pts',(-0.137757819841364,-0.117427728395404,
0.0310399036359917));
#17865=CARTESIAN_POINT('Ctrl Pts',(-0.174460933778308,0.0480767578110765,
0.0232799277269937));
#17866=CARTESIAN_POINT('Ctrl Pts',(-0.0581466660421577,0.171532975008042,
0.0155199518179959));
#17867=CARTESIAN_POINT('Ctrl Pts',(0.109502662757235,0.144085240745689,
0.00775997590899784));
#17868=CARTESIAN_POINT('Ctrl Pts',(0.156737212705124,0.0419221657566679,
0.00258665863633264));
#17869=CARTESIAN_POINT('Ctrl Pts',(0.15408394018464,-0.00816268198427004,
0.));
#17870=CARTESIAN_POINT('Ctrl Pts',(0.15408394018464,-0.00816268198427004,
0.));
#17871=CARTESIAN_POINT('Ctrl Pts',(0.153697863146473,0.00250812953454787,
1.45220469349306E-17));
#17872=CARTESIAN_POINT('Ctrl Pts',(0.152123106309386,0.0130673133993916,
-2.32988231788825E-17));
#17873=CARTESIAN_POINT('Ctrl Pts',(0.149466152202855,0.0233620190894148,
-6.07153216591882E-17));
#17874=CARTESIAN_POINT('Ctrl Pts',(0.14793019248835,0.0293132898222067,
-8.23454409684948E-17));
#17875=CARTESIAN_POINT('Ctrl Pts',(0.146031563681721,0.0351760135160456,
3.17823908273165E-17));
#17876=CARTESIAN_POINT('Ctrl Pts',(0.143784059453749,0.0409171473780902,
6.24500451351651E-17));
#17877=CARTESIAN_POINT('Ctrl Pts',(0.142595904075608,0.0439522291322952,
7.86626679846993E-17));
#17878=CARTESIAN_POINT('Ctrl Pts',(0.141309213132582,0.0469553015723855,
1.03399090950918E-16));
#17879=CARTESIAN_POINT('Ctrl Pts',(0.13992871365498,0.0499144025840292,
1.00613961606655E-16));
#17880=CARTESIAN_POINT('Ctrl Pts',(0.135493978469587,0.0594202586791481,
9.16669744478229E-17));
#17881=CARTESIAN_POINT('Ctrl Pts',(0.130119641392827,0.0684241765595774,
5.76730757846686E-17));
#17882=CARTESIAN_POINT('Ctrl Pts',(0.123887660540245,0.0767683201192124,
1.38777878078145E-16));
#17883=CARTESIAN_POINT('Ctrl Pts',(0.120656388342022,0.0810947453345699,
1.808305895663E-16));
#17884=CARTESIAN_POINT('Ctrl Pts',(0.117193874983239,0.0852432898306738,
1.062697842984E-16));
#17885=CARTESIAN_POINT('Ctrl Pts',(0.11350808038867,0.0891875047540603,
1.14491749414469E-16));
#17886=CARTESIAN_POINT('Ctrl Pts',(0.110158526423333,0.0927719043720516,
1.21963656801269E-16));
#17887=CARTESIAN_POINT('Ctrl Pts',(0.106618991420749,0.0961915975683434,
1.17223950247179E-16));
#17888=CARTESIAN_POINT('Ctrl Pts',(0.102922970874274,0.0994011657423757,
1.02348685082632E-16));
#17889=CARTESIAN_POINT('Ctrl Pts',(0.0973787571548163,0.104215676830788,
8.00350512245867E-17));
#17890=CARTESIAN_POINT('Ctrl Pts',(0.0914754811895955,0.108568278221023,
6.56075743842472E-17));
#17891=CARTESIAN_POINT('Ctrl Pts',(0.0852365492443714,0.11239450959967,
3.29597460435593E-17));
#17892=CARTESIAN_POINT('Ctrl Pts',(0.0787787796913796,0.116354950379705,
-7.26807264206779E-19));
#17893=CARTESIAN_POINT('Ctrl Pts',(0.0719608771003193,0.11975150351845,
7.81983513604452E-17));
#17894=CARTESIAN_POINT('Ctrl Pts',(0.0648645680501024,0.122569786811788,
1.05818132034585E-16));
#17895=CARTESIAN_POINT('Ctrl Pts',(0.0619760396963809,0.123716959397427,
1.17060669392563E-16));
#17896=CARTESIAN_POINT('Ctrl Pts',(0.0590419697559043,0.124767587801255,
-1.70921410850511E-17));
#17897=CARTESIAN_POINT('Ctrl Pts',(0.0560804949635964,0.12571697313192,
-8.67361737988404E-19));
#17898=CARTESIAN_POINT('Ctrl Pts',(0.0481895916857994,0.128246627558523,
4.23638569993146E-17));
#17899=CARTESIAN_POINT('Ctrl Pts',(0.040081547172159,0.13006877931966,2.48189907303608E-17));
#17900=CARTESIAN_POINT('Ctrl Pts',(0.0318655688619291,0.131172622122806,
0.));
#17901=CARTESIAN_POINT('Ctrl Pts',(0.0267717292715239,0.131856995664207,
-1.5387571972871E-17));
#17902=CARTESIAN_POINT('Ctrl Pts',(0.0216363184326117,0.132264755542675,
5.61228976213782E-17));
#17903=CARTESIAN_POINT('Ctrl Pts',(0.0164863123329273,0.132388468809724,
3.03576608295941E-17));
#17904=CARTESIAN_POINT('Ctrl Pts',(0.0120733572364389,0.13249447666326,
8.27985532573229E-18));
#17905=CARTESIAN_POINT('Ctrl Pts',(0.00764667637530932,0.132391154756805,
7.9933444120104E-17));
#17906=CARTESIAN_POINT('Ctrl Pts',(0.00324855819595315,0.132074892239241,
9.62771529167128E-17));
#17907=CARTESIAN_POINT('Ctrl Pts',(-0.00215998367955725,0.131685971569047,
1.16375665467493E-16));
#17908=CARTESIAN_POINT('Ctrl Pts',(-0.00753310453775717,0.130975837616781,
1.12286849362194E-16));
#17909=CARTESIAN_POINT('Ctrl Pts',(-0.0128378223015392,0.129936202211006,
1.27068494615301E-16));
#17910=CARTESIAN_POINT('Ctrl Pts',(-0.0180922709275414,0.128906418710228,
1.41710064449709E-16));
#17911=CARTESIAN_POINT('Ctrl Pts',(-0.023283936630727,0.12755123862641,
1.19281234835921E-16));
#17912=CARTESIAN_POINT('Ctrl Pts',(-0.028350637156304,0.125868914531291,
9.19403442267708E-17));
#17913=CARTESIAN_POINT('Ctrl Pts',(-0.0326437071621008,0.124443463179602,
6.87741127091605E-17));
#17914=CARTESIAN_POINT('Ctrl Pts',(-0.0368509055758185,0.122782751372096,
3.08039683582783E-17));
#17915=CARTESIAN_POINT('Ctrl Pts',(-0.0409513668396969,0.120880349084932,
-1.95156391047391E-18));
#17916=CARTESIAN_POINT('Ctrl Pts',(-0.0436523616789034,0.119627226953286,
-2.45035827619675E-17));
#17917=CARTESIAN_POINT('Ctrl Pts',(-0.0463070048384274,0.118269169850402,
-4.56986185075063E-18));
#17918=CARTESIAN_POINT('Ctrl Pts',(-0.0489111879062984,0.116810626195002,
-1.73472347597681E-18));
#17919=CARTESIAN_POINT('Ctrl Pts',(0.0958116152722397,0.0825211298936481,
0.24));
#17920=CARTESIAN_POINT('Ctrl Pts',(0.102494250906434,0.0762804363331629,
0.24));
#17921=CARTESIAN_POINT('Ctrl Pts',(0.108399952301676,0.0693089192431419,
0.24));
#17922=CARTESIAN_POINT('Ctrl Pts',(0.113520383394708,0.0617855200816623,
0.24));
#17923=CARTESIAN_POINT('Ctrl Pts',(0.11760088593285,0.0557900777417299,
0.24));
#17924=CARTESIAN_POINT('Ctrl Pts',(0.1211824537664,0.0494427873910869,0.24));
#17925=CARTESIAN_POINT('Ctrl Pts',(0.124247292533427,0.0428169095598754,
0.24));
#17926=CARTESIAN_POINT('Ctrl Pts',(0.125635784531567,0.0398151273949318,
0.24));
#17927=CARTESIAN_POINT('Ctrl Pts',(0.126914357096627,0.0367636074968772,
0.24));
#17928=CARTESIAN_POINT('Ctrl Pts',(0.128080244072735,0.0336751552254939,
0.24));
#17929=CARTESIAN_POINT('Ctrl Pts',(0.13155694143068,0.024465331227027,0.24));
#17930=CARTESIAN_POINT('Ctrl Pts',(0.134041462136676,0.0149150332268467,
0.24));
#17931=CARTESIAN_POINT('Ctrl Pts',(0.135496608205084,0.00520422800883078,
0.24));
#17932=CARTESIAN_POINT('Ctrl Pts',(0.136052940597398,0.00149158663520877,
0.24));
#17933=CARTESIAN_POINT('Ctrl Pts',(0.136458356591543,-0.00224482315054724,
0.24));
#17934=CARTESIAN_POINT('Ctrl Pts',(0.136708928272429,-0.00599574054845843,
0.24));
#17935=CARTESIAN_POINT('Ctrl Pts',(0.136894600108428,-0.00877514370161729,
0.24));
#17936=CARTESIAN_POINT('Ctrl Pts',(0.136994942037659,-0.0115613689854128,
0.24));
#17937=CARTESIAN_POINT('Ctrl Pts',(0.137008733057845,-0.0143405417274864,
0.24));
#17938=CARTESIAN_POINT('Ctrl Pts',(0.137045731231951,-0.0217964308202384,
0.24));
#17939=CARTESIAN_POINT('Ctrl Pts',(0.136462408227525,-0.0292204075226799,
0.24));
#17940=CARTESIAN_POINT('Ctrl Pts',(0.135240454646173,-0.0365388974416549,
0.24));
#17941=CARTESIAN_POINT('Ctrl Pts',(0.134058793448489,-0.0436160693529878,
0.24));
#17942=CARTESIAN_POINT('Ctrl Pts',(0.132280018312676,-0.050595007513092,
0.24));
#17943=CARTESIAN_POINT('Ctrl Pts',(0.129952822193542,-0.0574290655609092,
0.24));
#17944=CARTESIAN_POINT('Ctrl Pts',(0.128850070284018,-0.0606674134165377,
0.24));
#17945=CARTESIAN_POINT('Ctrl Pts',(0.127623182384127,-0.0638741644409745,
0.24));
#17946=CARTESIAN_POINT('Ctrl Pts',(0.126284110088584,-0.067028198101918,
0.24));
#17947=CARTESIAN_POINT('Ctrl Pts',(0.122654675969015,-0.0755769205431157,
0.24));
#17948=CARTESIAN_POINT('Ctrl Pts',(0.118195290975453,-0.0837663478860722,
0.24));
#17949=CARTESIAN_POINT('Ctrl Pts',(0.113014989178579,-0.0915013065162071,
0.24));
#17950=CARTESIAN_POINT('Ctrl Pts',(0.108985931714537,-0.0975172866704144,
0.24));
#17951=CARTESIAN_POINT('Ctrl Pts',(0.104519884911976,-0.103258562704539,
0.24));
#17952=CARTESIAN_POINT('Ctrl Pts',(0.0996546828651377,-0.108675969178894,
0.24));
#17953=CARTESIAN_POINT('Ctrl Pts',(0.0972822643803542,-0.11131765910988,
0.24));
#17954=CARTESIAN_POINT('Ctrl Pts',(0.09482095240722,-0.113875293456495,
0.24));
#17955=CARTESIAN_POINT('Ctrl Pts',(0.0922773332174137,-0.116342466058553,
0.24));
#17956=CARTESIAN_POINT('Ctrl Pts',(0.0868426048671788,-0.121613857680014,
0.24));
#17957=CARTESIAN_POINT('Ctrl Pts',(0.0810310485854155,-0.126474759557936,
0.24));
#17958=CARTESIAN_POINT('Ctrl Pts',(0.0748870600798396,-0.130870957562724,
0.24));
#17959=CARTESIAN_POINT('Ctrl Pts',(0.0715378781224404,-0.133267392228159,
0.24));
#17960=CARTESIAN_POINT('Ctrl Pts',(0.0680912231566627,-0.135524142754832,
0.24));
#17961=CARTESIAN_POINT('Ctrl Pts',(0.0645638484115253,-0.13762659390894,
0.24));
#17962=CARTESIAN_POINT('Ctrl Pts',(0.0598451535113139,-0.140439117742,0.24));
#17963=CARTESIAN_POINT('Ctrl Pts',(0.0549775790306604,-0.142978967531553,
0.24));
#17964=CARTESIAN_POINT('Ctrl Pts',(0.0499773507040556,-0.145225083935062,
0.24));
#17965=CARTESIAN_POINT('Ctrl Pts',(0.0466920976074369,-0.146700828718701,
0.24));
#17966=CARTESIAN_POINT('Ctrl Pts',(0.0433495270099635,-0.148049731670784,
0.24));
#17967=CARTESIAN_POINT('Ctrl Pts',(0.039956549802796,-0.149273502906639,
0.24));
#17968=CARTESIAN_POINT('Ctrl Pts',(-0.126296536029262,-6.10717992316628E-5,
0.159341967361942));
#17969=CARTESIAN_POINT('Ctrl Pts',(-0.12637083907321,-0.0163056929409037,
0.160361391877968));
#17970=CARTESIAN_POINT('Ctrl Pts',(-0.12344809088261,-0.0325245895549842,
0.161380816393994));
#17971=CARTESIAN_POINT('Ctrl Pts',(-0.117399968681154,-0.0474794518833934,
0.162400240910021));
#17972=CARTESIAN_POINT('Ctrl Pts',(-0.102053636235694,-0.0854254922118417,
0.164986899546353));
#17973=CARTESIAN_POINT('Ctrl Pts',(-0.0665853528586453,-0.115233359066084,
0.167573558182686));
#17974=CARTESIAN_POINT('Ctrl Pts',(-0.0265641275910804,-0.123819689910512,
0.170160216819019));
#17975=CARTESIAN_POINT('Ctrl Pts',(0.0134570976764845,-0.13240602075494,
0.172746875455351));
#17976=CARTESIAN_POINT('Ctrl Pts',(0.058031264834566,-0.119770815589554,
0.175333534091684));
#17977=CARTESIAN_POINT('Ctrl Pts',(0.0875924985281064,-0.0914586003428122,
0.177920192728017));
#17978=CARTESIAN_POINT('Ctrl Pts',(0.117153732221647,-0.0631463850960709,
0.180506851364349));
#17979=CARTESIAN_POINT('Ctrl Pts',(0.131702032450646,-0.0191571597679751,
0.183093510000682));
#17980=CARTESIAN_POINT('Ctrl Pts',(0.124851119980295,0.0211965060081854,
0.185680168637015));
#17981=CARTESIAN_POINT('Ctrl Pts',(0.118000207509943,0.0615501717843459,
0.188266827273347));
#17982=CARTESIAN_POINT('Ctrl Pts',(0.0897500823402403,0.0982682780085711,
0.19085348590968));
#17983=CARTESIAN_POINT('Ctrl Pts',(0.0525017161220023,0.115239608835997,
0.193440144546013));
#17984=CARTESIAN_POINT('Ctrl Pts',(0.0152533499037644,0.132210939663423,
0.196026803182345));
#17985=CARTESIAN_POINT('Ctrl Pts',(-0.030993257363009,0.129435495094051,
0.198613461818678));
#17986=CARTESIAN_POINT('Ctrl Pts',(-0.0659388717692058,0.108119484364762,
0.20120012045501));
#17987=CARTESIAN_POINT('Ctrl Pts',(-0.100884486175403,0.0868034736354726,
0.203786779091343));
#17988=CARTESIAN_POINT('Ctrl Pts',(-0.124529107721023,0.0469468967462671,
0.206373437727676));
#17989=CARTESIAN_POINT('Ctrl Pts',(-0.126492123469331,0.00606801008988057,
0.208960096364008));
#17990=CARTESIAN_POINT('Ctrl Pts',(-0.126588724127832,0.00405634646811867,
0.209087386696653));
#17991=CARTESIAN_POINT('Ctrl Pts',(-0.126632819376787,0.00204220716288977,
0.209214677029297));
#17992=CARTESIAN_POINT('Ctrl Pts',(-0.126625441102054,2.7778768752873E-5,
0.209341967361942));
#17993=CARTESIAN_POINT('Ctrl Pts',(-0.0398513841857245,-0.149064942821851,
0.24));
#17994=CARTESIAN_POINT('Ctrl Pts',(-0.0883048112969314,-0.136111285829332,
0.237413341363667));
#17995=CARTESIAN_POINT('Ctrl Pts',(-0.170871437255804,-0.0596187094618861,
0.232240024091002));
#17996=CARTESIAN_POINT('Ctrl Pts',(-0.145169204726118,0.108307533342445,
0.224480048182004));
#17997=CARTESIAN_POINT('Ctrl Pts',(0.00818767200092134,0.180778621679153,
0.216720072273006));
#17998=CARTESIAN_POINT('Ctrl Pts',(0.154249898498561,0.0947283641859207,
0.208960096364008));
#17999=CARTESIAN_POINT('Ctrl Pts',(0.164950538597243,-0.0745810526211722,
0.201200120455011));
#18000=CARTESIAN_POINT('Ctrl Pts',(0.0308106631569891,-0.178364693496558,
0.193440144546012));
#18001=CARTESIAN_POINT('Ctrl Pts',(-0.13036283225522,-0.125587074703769,
0.185680168637015));
#18002=CARTESIAN_POINT('Ctrl Pts',(-0.17709781441264,0.03745832727601,0.177920192728017));
#18003=CARTESIAN_POINT('Ctrl Pts',(-0.0683530255288039,0.167611467503216,
0.170160216819019));
#18004=CARTESIAN_POINT('Ctrl Pts',(0.100397202365132,0.150621028353064,
0.162400240910021));
#18005=CARTESIAN_POINT('Ctrl Pts',(0.18100910679194,0.00139719974911195,
0.154640265001023));
#18006=CARTESIAN_POINT('Ctrl Pts',(0.102711092909207,-0.149052183789333,
0.146880289092025));
#18007=CARTESIAN_POINT('Ctrl Pts',(-0.0657574679958034,-0.168648048308422,
0.139120313183027));
#18008=CARTESIAN_POINT('Ctrl Pts',(-0.176497206835689,-0.0401861834345609,
0.131360337274029));
#18009=CARTESIAN_POINT('Ctrl Pts',(-0.132288575936487,0.123555290563421,
0.123600361365031));
#18010=CARTESIAN_POINT('Ctrl Pts',(0.0280571680938306,0.178826694862324,
0.115840385456033));
#18011=CARTESIAN_POINT('Ctrl Pts',(0.163771354656592,0.0771047007047774,
0.108080409547035));
#18012=CARTESIAN_POINT('Ctrl Pts',(0.155709331479018,-0.0923080778690166,
0.100320433638038));
#18013=CARTESIAN_POINT('Ctrl Pts',(0.0109489686262093,-0.180682908560435,
0.0925604577290397));
#18014=CARTESIAN_POINT('Ctrl Pts',(-0.143423754439364,-0.110434756566834,
0.0848004818200417));
#18015=CARTESIAN_POINT('Ctrl Pts',(-0.17188331593326,0.0567648465404429,
0.0770405059110439));
#18016=CARTESIAN_POINT('Ctrl Pts',(-0.0494457976037486,0.174130301808973,
0.0692805300020459));
#18017=CARTESIAN_POINT('Ctrl Pts',(0.11640175885633,0.13862511662766,0.061520554093048));
#18018=CARTESIAN_POINT('Ctrl Pts',(0.18005704388064,-0.0185795878987759,
0.0537605781840501));
#18019=CARTESIAN_POINT('Ctrl Pts',(0.0856431484406112,-0.159474177462153,
0.0460006022750521));
#18020=CARTESIAN_POINT('Ctrl Pts',(-0.0839657292871194,-0.160363143120653,
0.0382406263660544));
#18021=CARTESIAN_POINT('Ctrl Pts',(-0.179844832231877,-0.0204718628801216,
0.0304806504570563));
#18022=CARTESIAN_POINT('Ctrl Pts',(-0.117866479118068,0.137399078213474,
0.0227206745480585));
#18023=CARTESIAN_POINT('Ctrl Pts',(0.0476444145610997,0.174632482457551,
0.0149606986390605));
#18024=CARTESIAN_POINT('Ctrl Pts',(0.171219786572432,0.0585809927800803,
0.00720072273006264));
#18025=CARTESIAN_POINT('Ctrl Pts',(0.144688050375066,-0.108949473877577,
-0.000559253178935319));
#18026=CARTESIAN_POINT('Ctrl Pts',(-0.0092814439579932,-0.180735423716049,
-0.00831922908793317));
#18027=CARTESIAN_POINT('Ctrl Pts',(-0.105867686800049,-0.122947365648507,
-0.0134925463605985));
#18028=CARTESIAN_POINT('Ctrl Pts',(-0.131895903200816,-0.0800747195988904,
-0.0160792049969312));
#18029=CARTESIAN_POINT('Ctrl Pts',(-0.0374537582415196,-0.140096572423086,
0.245359734998977));
#18030=CARTESIAN_POINT('Ctrl Pts',(-0.0829920245295529,-0.127922261611689,
0.242773076362644));
#18031=CARTESIAN_POINT('Ctrl Pts',(-0.160591096949962,-0.0560317985556137,
0.237599759089979));
#18032=CARTESIAN_POINT('Ctrl Pts',(-0.13643521822445,0.101791299158848,
0.229839783180981));
#18033=CARTESIAN_POINT('Ctrl Pts',(0.00769506740980954,0.1699022237233,
0.222079807271983));
#18034=CARTESIAN_POINT('Ctrl Pts',(0.144969579481095,0.0890291096113304,
0.214319831362985));
#18035=CARTESIAN_POINT('Ctrl Pts',(0.155026424317845,-0.0700939445729984,
0.206559855453987));
#18036=CARTESIAN_POINT('Ctrl Pts',(0.0289569648011409,-0.167633527556011,
0.19879987954499));
#18037=CARTESIAN_POINT('Ctrl Pts',(-0.122519659046519,-0.118031231043151,
0.191039903635991));
#18038=CARTESIAN_POINT('Ctrl Pts',(-0.166442869216287,0.0352046776440443,
0.183279927726994));
#18039=CARTESIAN_POINT('Ctrl Pts',(-0.064240621638164,0.157527260611955,
0.175519951817996));
#18040=CARTESIAN_POINT('Ctrl Pts',(0.0943568867767351,0.141559037340679,
0.167759975908998));
#18041=CARTESIAN_POINT('Ctrl Pts',(0.170118841887737,0.00131313836865665,
0.16));
#18042=CARTESIAN_POINT('Ctrl Pts',(0.0965315639882279,-0.140084581027326,
0.152240024091002));
#18043=CARTESIAN_POINT('Ctrl Pts',(-0.0618012237018238,-0.158501476380598,
0.144480048182004));
#18044=CARTESIAN_POINT('Ctrl Pts',(-0.165878396703103,-0.0377684145673052,
0.136720072273006));
#18045=CARTESIAN_POINT('Ctrl Pts',(-0.124329541933827,0.116121687534276,
0.128960096364008));
#18046=CARTESIAN_POINT('Ctrl Pts',(0.0263691315170036,0.168067732987372,
0.12120012045501));
#18047=CARTESIAN_POINT('Ctrl Pts',(0.153918185014798,0.0724657594331675,
0.113440144546012));
#18048=CARTESIAN_POINT('Ctrl Pts',(0.146341206869619,-0.0867544378416841,
0.105680168637015));
#18049=CARTESIAN_POINT('Ctrl Pts',(0.0102902328814698,-0.169812269106107,
0.0979201927280167));
#18050=CARTESIAN_POINT('Ctrl Pts',(-0.134794781526993,-0.103790539737311,
0.0901602168190187));
#18051=CARTESIAN_POINT('Ctrl Pts',(-0.161542096774173,0.0533496359633175,
0.0824002409100209));
#18052=CARTESIAN_POINT('Ctrl Pts',(-0.0464709316213242,0.163653894581969,
0.074640265001023));
#18053=CARTESIAN_POINT('Ctrl Pts',(0.109398542213106,0.130284849835523,
0.066880289092025));
#18054=CARTESIAN_POINT('Ctrl Pts',(0.16922405906302,-0.0174617621848401,
0.0591203131830272));
#18055=CARTESIAN_POINT('Ctrl Pts',(0.0804904984426183,-0.149879543972585,
0.0513603372740291));
#18056=CARTESIAN_POINT('Ctrl Pts',(-0.0789139998409189,-0.150715025739123,
0.0436003613650314));
#18057=CARTESIAN_POINT('Ctrl Pts',(-0.169024614954586,-0.0192401899891918,
0.0358403854560333));
#18058=CARTESIAN_POINT('Ctrl Pts',(-0.110775138777956,0.12913257502003,
0.0280804095470356));
#18059=CARTESIAN_POINT('Ctrl Pts',(0.0447779273164969,0.164125861942445,
0.0203204336380375));
#18060=CARTESIAN_POINT('Ctrl Pts',(0.16091848811479,0.0550565152494576,
0.0125604577290397));
#18061=CARTESIAN_POINT('Ctrl Pts',(0.135983012131502,-0.10239461786658,
0.00480048182004171));
#18062=CARTESIAN_POINT('Ctrl Pts',(-0.00872303347143,-0.169861624730324,
-0.00295949408895612));
#18063=CARTESIAN_POINT('Ctrl Pts',(-0.0994982439886826,-0.115550337924785,
-0.00813281136162148));
#18064=CARTESIAN_POINT('Ctrl Pts',(-0.123960494032221,-0.0752570895690155,
-0.0107194699979541));
#18065=CARTESIAN_POINT('Ctrl Pts',(-0.0350561322973148,-0.13112820202432,
0.250719469997954));
#18066=CARTESIAN_POINT('Ctrl Pts',(-0.0776792377621743,-0.119733237394047,
0.248132811361621));
#18067=CARTESIAN_POINT('Ctrl Pts',(-0.150310756644121,-0.0524448876493412,
0.242959494088956));
#18068=CARTESIAN_POINT('Ctrl Pts',(-0.127701231722781,0.0952750649752511,
0.235199518179958));
#18069=CARTESIAN_POINT('Ctrl Pts',(0.00720246281869772,0.159025825767447,
0.22743954227096));
#18070=CARTESIAN_POINT('Ctrl Pts',(0.135689260463629,0.08332985503674,0.219679566361962));
#18071=CARTESIAN_POINT('Ctrl Pts',(0.145102310038447,-0.0656068365248246,
0.211919590452964));
#18072=CARTESIAN_POINT('Ctrl Pts',(0.0271032664452926,-0.156902361615465,
0.204159614543967));
#18073=CARTESIAN_POINT('Ctrl Pts',(-0.114676485837817,-0.110475387382534,
0.196399638634969));
#18074=CARTESIAN_POINT('Ctrl Pts',(-0.155787924019933,0.0329510280120788,
0.188639662725971));
#18075=CARTESIAN_POINT('Ctrl Pts',(-0.0601282177475243,0.147443053720694,
0.180879686816973));
#18076=CARTESIAN_POINT('Ctrl Pts',(0.0883165711883383,0.132497046328295,
0.173119710907975));
#18077=CARTESIAN_POINT('Ctrl Pts',(0.159228576983534,0.00122907698820117,
0.165359734998977));
#18078=CARTESIAN_POINT('Ctrl Pts',(0.0903520350672485,-0.131116978265319,
0.157599759089979));
#18079=CARTESIAN_POINT('Ctrl Pts',(-0.0578449794078444,-0.148354904452775,
0.149839783180981));
#18080=CARTESIAN_POINT('Ctrl Pts',(-0.155259586570517,-0.0353506457000499,
0.142079807271983));
#18081=CARTESIAN_POINT('Ctrl Pts',(-0.116370507931168,0.108688084505131,
0.134319831362985));
#18082=CARTESIAN_POINT('Ctrl Pts',(0.0246810949401768,0.157308771112418,
0.126559855453988));
#18083=CARTESIAN_POINT('Ctrl Pts',(0.144065015373005,0.0678268181615582,
0.118799879544989));
#18084=CARTESIAN_POINT('Ctrl Pts',(0.13697308226022,-0.0812007978143519,
0.111039903635992));
#18085=CARTESIAN_POINT('Ctrl Pts',(0.00963149713673027,-0.15894162965178,
0.103279927726994));
#18086=CARTESIAN_POINT('Ctrl Pts',(-0.126165808614623,-0.0971463229077874,
0.0955199518179957));
#18087=CARTESIAN_POINT('Ctrl Pts',(-0.151200877615086,0.0499344253861922,
0.087759975908998));
#18088=CARTESIAN_POINT('Ctrl Pts',(-0.0434960656388994,0.153177487354966,
0.08));
#18089=CARTESIAN_POINT('Ctrl Pts',(0.102395325569881,0.121944583043386,
0.072240024091002));
#18090=CARTESIAN_POINT('Ctrl Pts',(0.158391074245402,-0.0163439364709043,
0.0644800481820042));
#18091=CARTESIAN_POINT('Ctrl Pts',(0.0753378484446251,-0.140284910483017,
0.0567200722730062));
#18092=CARTESIAN_POINT('Ctrl Pts',(-0.0738622703947183,-0.141066908357593,
0.0489600963640083));
#18093=CARTESIAN_POINT('Ctrl Pts',(-0.158204397677296,-0.018008517098262,
0.0412001204550104));
#18094=CARTESIAN_POINT('Ctrl Pts',(-0.103683798437843,0.120866071826586,
0.0334401445460125));
#18095=CARTESIAN_POINT('Ctrl Pts',(0.0419114400718942,0.153619241427338,
0.0256801686370146));
#18096=CARTESIAN_POINT('Ctrl Pts',(0.150617189657149,0.051532037718835,
0.0179201927280167));
#18097=CARTESIAN_POINT('Ctrl Pts',(0.127277973887939,-0.0958397618555833,
0.0101602168190187));
#18098=CARTESIAN_POINT('Ctrl Pts',(-0.00816462298486686,-0.1589878257446,
0.00240024091002091));
#18099=CARTESIAN_POINT('Ctrl Pts',(-0.0931288011773165,-0.108153310201063,
-0.00277307636264444));
#18100=CARTESIAN_POINT('Ctrl Pts',(-0.116025084863626,-0.0704394595391406,
-0.00535973499897709));
#18101=CARTESIAN_POINT('Ctrl Pts',(-0.0326585063531099,-0.122159831625555,
0.256079204996931));
#18102=CARTESIAN_POINT('Ctrl Pts',(-0.0723664509947957,-0.111544213176404,
0.253492546360598));
#18103=CARTESIAN_POINT('Ctrl Pts',(-0.140030416338279,-0.0488579767430688,
0.248319229087933));
#18104=CARTESIAN_POINT('Ctrl Pts',(-0.118967245221113,0.0887588307916541,
0.240559253178936));
#18105=CARTESIAN_POINT('Ctrl Pts',(0.00670985822758596,0.148149427811594,
0.232799277269937));
#18106=CARTESIAN_POINT('Ctrl Pts',(0.126408941446163,0.0776306004621497,
0.225039301360939));
#18107=CARTESIAN_POINT('Ctrl Pts',(0.13517819575905,-0.0611197284766509,
0.217279325451942));
#18108=CARTESIAN_POINT('Ctrl Pts',(0.0252495680894444,-0.146171195674918,
0.209519349542944));
#18109=CARTESIAN_POINT('Ctrl Pts',(-0.106833312629116,-0.102919543721916,
0.201759373633946));
#18110=CARTESIAN_POINT('Ctrl Pts',(-0.14513297882358,0.0306973783801131,
0.193999397724948));
#18111=CARTESIAN_POINT('Ctrl Pts',(-0.0560158138568844,0.137358846829434,
0.18623942181595));
#18112=CARTESIAN_POINT('Ctrl Pts',(0.0822762555999414,0.12343505531591,
0.178479445906952));
#18113=CARTESIAN_POINT('Ctrl Pts',(0.148338312079331,0.00114501560774606,
0.170719469997954));
#18114=CARTESIAN_POINT('Ctrl Pts',(0.0841725061462688,-0.122149375503312,
0.162959494088956));
#18115=CARTESIAN_POINT('Ctrl Pts',(-0.0538887351138648,-0.138208332524951,
0.155199518179959));
#18116=CARTESIAN_POINT('Ctrl Pts',(-0.144640776437932,-0.0329328768327946,
0.14743954227096));
#18117=CARTESIAN_POINT('Ctrl Pts',(-0.108411473928508,0.101254481475986,
0.139679566361963));
#18118=CARTESIAN_POINT('Ctrl Pts',(0.0229930583633497,0.146549809237466,
0.131919590452964));
#18119=CARTESIAN_POINT('Ctrl Pts',(0.134211845731212,0.0631878768899486,
0.124159614543967));
#18120=CARTESIAN_POINT('Ctrl Pts',(0.127604957650822,-0.0756471577870196,
0.116399638634969));
#18121=CARTESIAN_POINT('Ctrl Pts',(0.00897276139199077,-0.148070990197453,
0.108639662725971));
#18122=CARTESIAN_POINT('Ctrl Pts',(-0.117536835702253,-0.0905021060782641,
0.100879686816973));
#18123=CARTESIAN_POINT('Ctrl Pts',(-0.140859658455999,0.0465192148090667,
0.0931197109079749));
#18124=CARTESIAN_POINT('Ctrl Pts',(-0.0405211996564747,0.142701080127962,
0.0853597349989771));
#18125=CARTESIAN_POINT('Ctrl Pts',(0.0953921089266558,0.113604316251249,
0.077599759089979));
#18126=CARTESIAN_POINT('Ctrl Pts',(0.147558089427783,-0.0152261107569683,
0.0698397831809813));
#18127=CARTESIAN_POINT('Ctrl Pts',(0.070185198446632,-0.130690276993449,
0.0620798072719832));
#18128=CARTESIAN_POINT('Ctrl Pts',(-0.0688105409485176,-0.131418790976063,
0.0543198313629854));
#18129=CARTESIAN_POINT('Ctrl Pts',(-0.147384180400005,-0.0167768442073323,
0.0465598554539874));
#18130=CARTESIAN_POINT('Ctrl Pts',(-0.0965924580977301,0.112599568633142,
0.0387998795449896));
#18131=CARTESIAN_POINT('Ctrl Pts',(0.0390449528272914,0.143112620912232,
0.0310399036359916));
#18132=CARTESIAN_POINT('Ctrl Pts',(0.140315891199508,0.0480075601882123,
0.0232799277269937));
#18133=CARTESIAN_POINT('Ctrl Pts',(0.118572935644375,-0.0892849058445864,
0.0155199518179958));
#18134=CARTESIAN_POINT('Ctrl Pts',(-0.00760621249830358,-0.148114026758875,
0.00775997590899793));
#18135=CARTESIAN_POINT('Ctrl Pts',(-0.0867593583659504,-0.100756282477341,
0.00258665863633259));
#18136=CARTESIAN_POINT('Ctrl Pts',(-0.108089675695031,-0.0656218295092657,
-5.55111512312578E-17));
#18137=CARTESIAN_POINT('Ctrl Pts',(-0.108089675695031,-0.0656218295092657,
-5.55111512312578E-17));
#18138=CARTESIAN_POINT('Ctrl Pts',(-0.104219465379748,-0.0739058869203245,
-4.02841154597017E-17));
#18139=CARTESIAN_POINT('Ctrl Pts',(-0.0994141168358061,-0.0816768736924768,
-5.16144647363644E-17));
#18140=CARTESIAN_POINT('Ctrl Pts',(-0.0938412360364922,-0.088871564406415,
-3.81639164714898E-17));
#18141=CARTESIAN_POINT('Ctrl Pts',(-0.0894001862863345,-0.094605040600905,
-2.74451237748006E-17));
#18142=CARTESIAN_POINT('Ctrl Pts',(-0.0844703330957707,-0.0999727304469881,
3.12377098840079E-17));
#18143=CARTESIAN_POINT('Ctrl Pts',(-0.0791158513129458,-0.104935071387697,
-1.21430643318376E-17));
#18144=CARTESIAN_POINT('Ctrl Pts',(-0.0766900604813501,-0.107183206995485,
-3.17962611543325E-17));
#18145=CARTESIAN_POINT('Ctrl Pts',(-0.0741829996358932,-0.109342173006691,
4.83248416902999E-17));
#18146=CARTESIAN_POINT('Ctrl Pts',(-0.0716059924168524,-0.111405381598006,
5.3776427755281E-17));
#18147=CARTESIAN_POINT('Ctrl Pts',(-0.0639212992135713,-0.117557915794061,
7.00331794132204E-17));
#18148=CARTESIAN_POINT('Ctrl Pts',(-0.0556061968393146,-0.12287204611112,
-5.69073736333764E-18));
#18149=CARTESIAN_POINT('Ctrl Pts',(-0.0468203466856493,-0.127256781127915,
5.55111512312578E-17));
#18150=CARTESIAN_POINT('Ctrl Pts',(-0.0434613267337519,-0.12893315986732,
7.89099528597243E-17));
#18151=CARTESIAN_POINT('Ctrl Pts',(-0.0400330653128497,-0.130473352587733,
3.97002991909352E-17));
#18152=CARTESIAN_POINT('Ctrl Pts',(-0.0365431560942257,-0.131870761756357,
6.59194920871187E-17));
#18153=CARTESIAN_POINT('Ctrl Pts',(-0.0339571636773035,-0.13290622981212,
8.5347686277821E-17));
#18154=CARTESIAN_POINT('Ctrl Pts',(-0.0313383144727484,-0.133862652235137,
-2.74403076010104E-17));
#18155=CARTESIAN_POINT('Ctrl Pts',(-0.0286994266230122,-0.134734580282325,
-2.42861286636753E-17));
#18156=CARTESIAN_POINT('Ctrl Pts',(-0.0216199050576346,-0.137073760181214,
-1.58242011095522E-17));
#18157=CARTESIAN_POINT('Ctrl Pts',(-0.0143790427459088,-0.138813119073991,
5.80198461902811E-17));
#18158=CARTESIAN_POINT('Ctrl Pts',(-0.0070411538297537,-0.139912507657099,
6.93889390390723E-17));
#18159=CARTESIAN_POINT('Ctrl Pts',(5.47883476400097E-5,-0.140975646920361,
8.02325614020808E-17));
#18160=CARTESIAN_POINT('Ctrl Pts',(0.00724182591717642,-0.141440539972256,
1.32011341321413E-16));
#18161=CARTESIAN_POINT('Ctrl Pts',(0.0144605478337719,-0.141339082434075,
1.61329283265843E-16));
#18162=CARTESIAN_POINT('Ctrl Pts',(0.0178811722145177,-0.141291006315792,
1.75221724083914E-16));
#18163=CARTESIAN_POINT('Ctrl Pts',(0.021310106848269,-0.141115105569205,
1.85534911235541E-16));
#18164=CARTESIAN_POINT('Ctrl Pts',(0.0247235715439624,-0.140816220288761,
1.71737624121704E-16));
#18165=CARTESIAN_POINT('Ctrl Pts',(0.0339754553361668,-0.140006119078294,
1.34341339582434E-16));
#18166=CARTESIAN_POINT('Ctrl Pts',(0.0431421008898472,-0.138295657968001,
8.04496487960062E-17));
#18167=CARTESIAN_POINT('Ctrl Pts',(0.0520992976556894,-0.135759125106636,
3.20923843055709E-17));
#18168=CARTESIAN_POINT('Ctrl Pts',(0.0590658916121619,-0.13378629867842,
-5.518202506064E-18));
#18169=CARTESIAN_POINT('Ctrl Pts',(0.0659062642374416,-0.131312982137409,
7.87850579480063E-17));
#18170=CARTESIAN_POINT('Ctrl Pts',(0.0725619642951071,-0.128359965266718,
7.63278329429795E-17));
#18171=CARTESIAN_POINT('Ctrl Pts',(0.0758074813473741,-0.126919986522721,
7.51296170399226E-17));
#18172=CARTESIAN_POINT('Ctrl Pts',(0.0790005264283722,-0.125369490597537,
8.38688896655138E-17));
#18173=CARTESIAN_POINT('Ctrl Pts',(0.0821329715644795,-0.123712761836801,
7.24247051220317E-17));
#18174=CARTESIAN_POINT('Ctrl Pts',(0.0888257654942848,-0.120172989003949,
4.79730178566093E-17));
#18175=CARTESIAN_POINT('Ctrl Pts',(0.0952446087626691,-0.116147988031934,
8.96774285244103E-17));
#18176=CARTESIAN_POINT('Ctrl Pts',(0.101324221742587,-0.111663228753314,
8.28330459778925E-17));
#18177=CARTESIAN_POINT('Ctrl Pts',(0.104638321741973,-0.109218510516871,
7.91020571356516E-17));
#18178=CARTESIAN_POINT('Ctrl Pts',(0.107849695272814,-0.106637925639498,
3.17151869302413E-17));
#18179=CARTESIAN_POINT('Ctrl Pts',(0.110939265073957,-0.10393289123317,
1.53956708492942E-17));
#18180=CARTESIAN_POINT('Ctrl Pts',(0.115072333360666,-0.100314234708527,
-6.43574216607592E-18));
#18181=CARTESIAN_POINT('Ctrl Pts',(0.118992075260627,-0.0964697210975667,
5.54296751400654E-17));
#18182=CARTESIAN_POINT('Ctrl Pts',(0.122673447199167,-0.0924082746861152,
3.52365706057789E-17));
#18183=CARTESIAN_POINT('Ctrl Pts',(0.125092164655522,-0.0897398425098966,
2.31620156359627E-17));
#18184=CARTESIAN_POINT('Ctrl Pts',(0.127407959881093,-0.0869777021544565,
-4.01489640485901E-17));
#18185=CARTESIAN_POINT('Ctrl Pts',(0.129620323775263,-0.0841289546921697,
-3.98986399474666E-17));
#18186=CARTESIAN_POINT('Ctrl Pts',(-0.126471935391749,0.000101176582396995,
0.195658032638058));
#18187=CARTESIAN_POINT('Ctrl Pts',(-0.126547267107008,0.00888033934128026,
0.195105154333688));
#18188=CARTESIAN_POINT('Ctrl Pts',(-0.125707148272093,0.0176451944231377,
0.194552276029318));
#18189=CARTESIAN_POINT('Ctrl Pts',(-0.12389684029672,0.0262048027713284,
0.193999397724948));
#18190=CARTESIAN_POINT('Ctrl Pts',(-0.115427257168015,0.0662512011965534,
0.191412739088615));
#18191=CARTESIAN_POINT('Ctrl Pts',(-0.0857215355124495,0.101805024012994,
0.188826080452282));
#18192=CARTESIAN_POINT('Ctrl Pts',(-0.0478199964418627,0.117261303502293,
0.18623942181595));
#18193=CARTESIAN_POINT('Ctrl Pts',(-0.0099184573712758,0.132717582991593,
0.183652763179617));
#18194=CARTESIAN_POINT('Ctrl Pts',(0.0361788991143328,0.128076319153751,
0.181066104543285));
#18195=CARTESIAN_POINT('Ctrl Pts',(0.070237920103702,0.105374013950137,
0.178479445906952));
#18196=CARTESIAN_POINT('Ctrl Pts',(0.104296941093071,0.0826717087465222,
0.175892787270619));
#18197=CARTESIAN_POINT('Ctrl Pts',(0.126317626586201,0.0419083621771342,
0.173306128634287));
#18198=CARTESIAN_POINT('Ctrl Pts',(0.126633668343922,0.000977623707263797,
0.170719469997954));
#18199=CARTESIAN_POINT('Ctrl Pts',(0.126949710101644,-0.0399531147626067,
0.168132811361621));
#18200=CARTESIAN_POINT('Ctrl Pts',(0.105561108123956,-0.08105124513296,
0.165546152725289));
#18201=CARTESIAN_POINT('Ctrl Pts',(0.0718566002584231,-0.104276803155076,
0.162959494088956));
#18202=CARTESIAN_POINT('Ctrl Pts',(0.0381520923928904,-0.127502361177192,
0.160372835452623));
#18203=CARTESIAN_POINT('Ctrl Pts',(-0.00786832136048696,-0.132855346851071,
0.157786176816291));
#18204=CARTESIAN_POINT('Ctrl Pts',(-0.0460038684578537,-0.117985930405985,
0.155199518179958));
#18205=CARTESIAN_POINT('Ctrl Pts',(-0.0841394155552204,-0.103116513960899,
0.152612859543626));
#18206=CARTESIAN_POINT('Ctrl Pts',(-0.114390095996576,-0.0680246953968468,
0.150026200907293));
#18207=CARTESIAN_POINT('Ctrl Pts',(-0.12347721913235,-0.0281142263966907,
0.14743954227096));
#18208=CARTESIAN_POINT('Ctrl Pts',(-0.125563410841138,-0.018951712774069,
0.14684570572666));
#18209=CARTESIAN_POINT('Ctrl Pts',(-0.126534167537385,-0.00953522996602069,
0.146251869182359));
#18210=CARTESIAN_POINT('Ctrl Pts',(-0.126453631260982,-0.000102348163238207,
0.145658032638058));
#18211=CARTESIAN_POINT('Ctrl Pts',(-0.0398513841857245,-0.149064942821851,
0.24));
#18212=CARTESIAN_POINT('Ctrl Pts',(-0.0498806325786677,-0.145400296738327,
0.24));
#18213=CARTESIAN_POINT('Ctrl Pts',(-0.0594363948008725,-0.140639648297949,
0.24));
#18214=CARTESIAN_POINT('Ctrl Pts',(-0.0684062055177017,-0.134931499399492,
0.24));
#18215=CARTESIAN_POINT('Ctrl Pts',(-0.0735915624001909,-0.131631676235849,
0.24));
#18216=CARTESIAN_POINT('Ctrl Pts',(-0.0785806353345173,-0.128014298080738,
0.24));
#18217=CARTESIAN_POINT('Ctrl Pts',(-0.0833462611484583,-0.124102693747304,
0.24));
#18218=CARTESIAN_POINT('Ctrl Pts',(-0.0858656342542594,-0.122034803580736,
0.24));
#18219=CARTESIAN_POINT('Ctrl Pts',(-0.0883241156266364,-0.11988309220465,
0.24));
#18220=CARTESIAN_POINT('Ctrl Pts',(-0.0907117892851122,-0.117655751751618,
0.24));
#18221=CARTESIAN_POINT('Ctrl Pts',(-0.0983819858496404,-0.110500611839494,
0.24));
#18222=CARTESIAN_POINT('Ctrl Pts',(-0.105284458416918,-0.102606966330569,
0.24));
#18223=CARTESIAN_POINT('Ctrl Pts',(-0.111294422020379,-0.0941015332659665,
0.24));
#18224=CARTESIAN_POINT('Ctrl Pts',(-0.114410577497229,-0.0896914812962706,
0.24));
#18225=CARTESIAN_POINT('Ctrl Pts',(-0.117286101138547,-0.0851164738413172,
0.24));
#18226=CARTESIAN_POINT('Ctrl Pts',(-0.119898298320422,-0.0803922539627851,
0.24));
#18227=CARTESIAN_POINT('Ctrl Pts',(-0.1222721977331,-0.0760990011896685,
0.24));
#18228=CARTESIAN_POINT('Ctrl Pts',(-0.124430744329062,-0.0716759619599862,
0.24));
#18229=CARTESIAN_POINT('Ctrl Pts',(-0.126341093034125,-0.0671690272221462,
0.24));
#18230=CARTESIAN_POINT('Ctrl Pts',(-0.129206708925078,-0.060408406100978,
0.24));
#18231=CARTESIAN_POINT('Ctrl Pts',(-0.131522065955468,-0.0534490321795157,
0.24));
#18232=CARTESIAN_POINT('Ctrl Pts',(-0.133233091500091,-0.0463330844490581,
0.24));
#18233=CARTESIAN_POINT('Ctrl Pts',(-0.135004134506116,-0.0389675313754268,
0.24));
#18234=CARTESIAN_POINT('Ctrl Pts',(-0.136127599829873,-0.0314337185245799,
0.24));
#18235=CARTESIAN_POINT('Ctrl Pts',(-0.136615064298196,-0.0238138180582873,
0.24));
#18236=CARTESIAN_POINT('Ctrl Pts',(-0.136813484749433,-0.0207121682209076,
0.24));
#18237=CARTESIAN_POINT('Ctrl Pts',(-0.136906013213758,-0.0175970392000076,
0.24));
#18238=CARTESIAN_POINT('Ctrl Pts',(-0.136893785357156,-0.0144871321155608,
0.24));
#18239=CARTESIAN_POINT('Ctrl Pts',(-0.136861203984761,-0.00620072149302863,
0.24));
#18240=CARTESIAN_POINT('Ctrl Pts',(-0.136088646936857,0.00207357465703332,
0.24));
#18241=CARTESIAN_POINT('Ctrl Pts',(-0.134599584032292,0.0102285531249486,
0.24));
#18242=CARTESIAN_POINT('Ctrl Pts',(-0.133676409755049,0.0152843948425598,
0.24));
#18243=CARTESIAN_POINT('Ctrl Pts',(-0.132477333465274,0.0202942984003417,
0.24));
#18244=CARTESIAN_POINT('Ctrl Pts',(-0.131003622030167,0.0252303138624672,
0.24));
#18245=CARTESIAN_POINT('Ctrl Pts',(-0.129740734874544,0.029460199292259,
0.24));
#18246=CARTESIAN_POINT('Ctrl Pts',(-0.128274507607502,0.0336384499732856,
0.24));
#18247=CARTESIAN_POINT('Ctrl Pts',(-0.126614574688298,0.0377237273426867,
0.24));
#18248=CARTESIAN_POINT('Ctrl Pts',(-0.124573382985647,0.042747324485064,
0.24));
#18249=CARTESIAN_POINT('Ctrl Pts',(-0.122237651925267,0.0476379767326878,
0.24));
#18250=CARTESIAN_POINT('Ctrl Pts',(-0.119609691052418,0.0523617558795304,
0.24));
#18251=CARTESIAN_POINT('Ctrl Pts',(-0.117006563775536,0.0570408964535612,
0.24));
#18252=CARTESIAN_POINT('Ctrl Pts',(-0.114113358229268,0.0615597689541448,
0.24));
#18253=CARTESIAN_POINT('Ctrl Pts',(-0.110947628485839,0.0658586917144141,
0.24));
#18254=CARTESIAN_POINT('Ctrl Pts',(-0.108265305855902,0.0695011687224882,
0.24));
#18255=CARTESIAN_POINT('Ctrl Pts',(-0.105385772272888,0.0729892759232728,
0.24));
#18256=CARTESIAN_POINT('Ctrl Pts',(-0.102309360287629,0.0763011815833395,
0.24));
#18257=CARTESIAN_POINT('Ctrl Pts',(-0.100282916666232,0.0784827457339379,
0.24));
#18258=CARTESIAN_POINT('Ctrl Pts',(-0.0981709975111385,0.0805877996091198,
0.24));
#18259=CARTESIAN_POINT('Ctrl Pts',(-0.0959791030802606,0.0826138105732947,
0.24));
#18260=CARTESIAN_POINT('Origin',(0.,0.,0.24));
#18261=CARTESIAN_POINT('',(0.158771324027147,-0.275,0.24));
#18262=CARTESIAN_POINT('',(0.317542648054294,0.,0.24));
#18263=CARTESIAN_POINT('',(0.158771324027147,-0.275,0.24));
#18264=CARTESIAN_POINT('',(0.158771324027147,0.275,0.24));
#18265=CARTESIAN_POINT('',(0.317542648054294,0.,0.24));
#18266=CARTESIAN_POINT('',(-0.158771324027147,0.275,0.24));
#18267=CARTESIAN_POINT('',(0.158771324027147,0.275,0.24));
#18268=CARTESIAN_POINT('',(-0.317542648054294,5.55111512312578E-17,0.24));
#18269=CARTESIAN_POINT('',(-0.158771324027147,0.275,0.24));
#18270=CARTESIAN_POINT('',(-0.158771324027147,-0.275,0.24));
#18271=CARTESIAN_POINT('',(-0.317542648054294,3.88877587532466E-17,0.24));
#18272=CARTESIAN_POINT('',(-0.158771324027147,-0.275,0.24));
#18273=CARTESIAN_POINT('Origin',(0.,0.,0.12));
#18274=CARTESIAN_POINT('Origin',(-0.158771324027147,-0.275,0.));
#18275=CARTESIAN_POINT('',(-0.158771324027147,-0.275,0.));
#18276=CARTESIAN_POINT('',(0.158771324027147,-0.275,0.));
#18277=CARTESIAN_POINT('',(-0.158771324027147,-0.275,0.));
#18278=CARTESIAN_POINT('',(0.158771324027147,-0.275,0.));
#18279=CARTESIAN_POINT('',(-0.158771324027147,-0.275,0.));
#18280=CARTESIAN_POINT('Origin',(-0.317542648054294,3.88877587532466E-17,
0.));
#18281=CARTESIAN_POINT('',(-0.317542648054294,3.88877587532466E-17,0.));
#18282=CARTESIAN_POINT('',(-0.317542648054294,3.88877587532466E-17,0.));
#18283=CARTESIAN_POINT('',(-0.317542648054294,3.88877587532466E-17,0.));
#18284=CARTESIAN_POINT('Origin',(-0.158771324027147,0.275,0.));
#18285=CARTESIAN_POINT('',(-0.158771324027147,0.275,0.));
#18286=CARTESIAN_POINT('',(-0.158771324027147,0.275,0.));
#18287=CARTESIAN_POINT('',(-0.158771324027147,0.275,0.));
#18288=CARTESIAN_POINT('Origin',(0.158771324027147,0.275,0.));
#18289=CARTESIAN_POINT('',(0.158771324027147,0.275,0.));
#18290=CARTESIAN_POINT('',(0.158771324027147,0.275,0.));
#18291=CARTESIAN_POINT('',(0.158771324027147,0.275,0.));
#18292=CARTESIAN_POINT('Origin',(0.317542648054294,0.,0.));
#18293=CARTESIAN_POINT('',(0.317542648054294,0.,0.));
#18294=CARTESIAN_POINT('',(0.317542648054294,0.,0.));
#18295=CARTESIAN_POINT('',(0.317542648054294,0.,0.));
#18296=CARTESIAN_POINT('Origin',(0.158771324027147,-0.275,0.));
#18297=CARTESIAN_POINT('',(0.158771324027147,-0.275,0.));
#18298=CARTESIAN_POINT('Origin',(0.,0.,0.));
#18299=CARTESIAN_POINT('',(0.,0.,0.));
#18300=CARTESIAN_POINT('',(0.,0.,0.));
#18301=CARTESIAN_POINT('',(0.,0.,0.));
#18302=CARTESIAN_POINT('',(2.,0.,0.6));
#18303=CARTESIAN_POINT('',(2.,0.,-0.84));
#18304=CARTESIAN_POINT('',(0.,0.,0.));
#18305=CARTESIAN_POINT('',(10.,0.,0.6));
#18306=CARTESIAN_POINT('',(10.,0.,-0.84));
#18307=CARTESIAN_POINT('',(0.,0.,0.));
#18308=CARTESIAN_POINT('Origin',(0.,0.,0.));
#18309=CARTESIAN_POINT('',(-0.41,-5.02105187650415E-17,0.1));
#18310=CARTESIAN_POINT('Origin',(0.,0.,0.1));
#18311=CARTESIAN_POINT('',(-0.41,-5.02105187650415E-17,0.));
#18312=CARTESIAN_POINT('',(-0.41,-5.02105187650415E-17,0.));
#18313=CARTESIAN_POINT('Origin',(0.,0.,0.));
#18314=CARTESIAN_POINT('Origin',(0.,0.,0.));
#18315=CARTESIAN_POINT('',(-0.6,-7.34788079488412E-17,0.1));
#18316=CARTESIAN_POINT('Origin',(0.,0.,0.1));
#18317=CARTESIAN_POINT('',(-0.6,-7.34788079488412E-17,0.));
#18318=CARTESIAN_POINT('',(-0.6,-7.34788079488412E-17,0.));
#18319=CARTESIAN_POINT('Origin',(0.,0.,0.));
#18320=CARTESIAN_POINT('Origin',(0.,0.,0.1));
#18321=CARTESIAN_POINT('Origin',(0.,0.,0.));
#18322=CARTESIAN_POINT('',(0.,0.,0.));
#18323=CARTESIAN_POINT('',(4.,-2.5,0.3));
#18324=CARTESIAN_POINT('',(0.,0.,0.));
#18325=CARTESIAN_POINT('',(0.,0.,0.));
#18326=CARTESIAN_POINT('',(0.,0.,0.6));
#18327=CARTESIAN_POINT('',(0.,0.,0.7));
#18328=CARTESIAN_POINT('',(4.,2.5,-0.3));
#18329=CARTESIAN_POINT('',(0.,0.,-0.7));
#18330=UNCERTAINTY_MEASURE_WITH_UNIT(LENGTH_MEASURE(0.001),#18354,
'DISTANCE_ACCURACY_VALUE',
'Maximum model space distance between geometric entities at asserted c
onnectivities');
#18331=UNCERTAINTY_MEASURE_WITH_UNIT(LENGTH_MEASURE(0.001),#18354,
'DISTANCE_ACCURACY_VALUE',
'Maximum model space distance between geometric entities at asserted c
onnectivities');
#18332=UNCERTAINTY_MEASURE_WITH_UNIT(LENGTH_MEASURE(0.001),#18354,
'DISTANCE_ACCURACY_VALUE',
'Maximum model space distance between geometric entities at asserted c
onnectivities');
#18333=UNCERTAINTY_MEASURE_WITH_UNIT(LENGTH_MEASURE(0.001),#18354,
'DISTANCE_ACCURACY_VALUE',
'Maximum model space distance between geometric entities at asserted c
onnectivities');
#18334=UNCERTAINTY_MEASURE_WITH_UNIT(LENGTH_MEASURE(0.001),#18354,
'DISTANCE_ACCURACY_VALUE',
'Maximum model space distance between geometric entities at asserted c
onnectivities');
#18335=UNCERTAINTY_MEASURE_WITH_UNIT(LENGTH_MEASURE(0.001),#18354,
'DISTANCE_ACCURACY_VALUE',
'Maximum model space distance between geometric entities at asserted c
onnectivities');
#18336=UNCERTAINTY_MEASURE_WITH_UNIT(LENGTH_MEASURE(0.001),#18354,
'DISTANCE_ACCURACY_VALUE',
'Maximum model space distance between geometric entities at asserted c
onnectivities');
#18337=UNCERTAINTY_MEASURE_WITH_UNIT(LENGTH_MEASURE(0.001),#18354,
'DISTANCE_ACCURACY_VALUE',
'Maximum model space distance between geometric entities at asserted c
onnectivities');
#18338=UNCERTAINTY_MEASURE_WITH_UNIT(LENGTH_MEASURE(0.001),#18354,
'DISTANCE_ACCURACY_VALUE',
'Maximum model space distance between geometric entities at asserted c
onnectivities');
#18339=UNCERTAINTY_MEASURE_WITH_UNIT(LENGTH_MEASURE(0.001),#18354,
'DISTANCE_ACCURACY_VALUE',
'Maximum model space distance between geometric entities at asserted c
onnectivities');
#18340=UNCERTAINTY_MEASURE_WITH_UNIT(LENGTH_MEASURE(0.001),#18354,
'DISTANCE_ACCURACY_VALUE',
'Maximum model space distance between geometric entities at asserted c
onnectivities');
#18341=UNCERTAINTY_MEASURE_WITH_UNIT(LENGTH_MEASURE(0.001),#18354,
'DISTANCE_ACCURACY_VALUE',
'Maximum model space distance between geometric entities at asserted c
onnectivities');
#18342=(
GEOMETRIC_REPRESENTATION_CONTEXT(3)
GLOBAL_UNCERTAINTY_ASSIGNED_CONTEXT((#18330))
GLOBAL_UNIT_ASSIGNED_CONTEXT((#18354,#18356,#18357))
REPRESENTATION_CONTEXT('','3D')
);
#18343=(
GEOMETRIC_REPRESENTATION_CONTEXT(3)
GLOBAL_UNCERTAINTY_ASSIGNED_CONTEXT((#18331))
GLOBAL_UNIT_ASSIGNED_CONTEXT((#18354,#18356,#18357))
REPRESENTATION_CONTEXT('','3D')
);
#18344=(
GEOMETRIC_REPRESENTATION_CONTEXT(3)
GLOBAL_UNCERTAINTY_ASSIGNED_CONTEXT((#18332))
GLOBAL_UNIT_ASSIGNED_CONTEXT((#18354,#18356,#18357))
REPRESENTATION_CONTEXT('','3D')
);
#18345=(
GEOMETRIC_REPRESENTATION_CONTEXT(3)
GLOBAL_UNCERTAINTY_ASSIGNED_CONTEXT((#18333))
GLOBAL_UNIT_ASSIGNED_CONTEXT((#18354,#18356,#18357))
REPRESENTATION_CONTEXT('','3D')
);
#18346=(
GEOMETRIC_REPRESENTATION_CONTEXT(3)
GLOBAL_UNCERTAINTY_ASSIGNED_CONTEXT((#18334))
GLOBAL_UNIT_ASSIGNED_CONTEXT((#18354,#18356,#18357))
REPRESENTATION_CONTEXT('','3D')
);
#18347=(
GEOMETRIC_REPRESENTATION_CONTEXT(3)
GLOBAL_UNCERTAINTY_ASSIGNED_CONTEXT((#18335))
GLOBAL_UNIT_ASSIGNED_CONTEXT((#18354,#18356,#18357))
REPRESENTATION_CONTEXT('','3D')
);
#18348=(
GEOMETRIC_REPRESENTATION_CONTEXT(3)
GLOBAL_UNCERTAINTY_ASSIGNED_CONTEXT((#18336))
GLOBAL_UNIT_ASSIGNED_CONTEXT((#18354,#18356,#18357))
REPRESENTATION_CONTEXT('','3D')
);
#18349=(
GEOMETRIC_REPRESENTATION_CONTEXT(3)
GLOBAL_UNCERTAINTY_ASSIGNED_CONTEXT((#18337))
GLOBAL_UNIT_ASSIGNED_CONTEXT((#18354,#18356,#18357))
REPRESENTATION_CONTEXT('','3D')
);
#18350=(
GEOMETRIC_REPRESENTATION_CONTEXT(3)
GLOBAL_UNCERTAINTY_ASSIGNED_CONTEXT((#18338))
GLOBAL_UNIT_ASSIGNED_CONTEXT((#18354,#18356,#18357))
REPRESENTATION_CONTEXT('','3D')
);
#18351=(
GEOMETRIC_REPRESENTATION_CONTEXT(3)
GLOBAL_UNCERTAINTY_ASSIGNED_CONTEXT((#18339))
GLOBAL_UNIT_ASSIGNED_CONTEXT((#18354,#18356,#18357))
REPRESENTATION_CONTEXT('','3D')
);
#18352=(
GEOMETRIC_REPRESENTATION_CONTEXT(3)
GLOBAL_UNCERTAINTY_ASSIGNED_CONTEXT((#18340))
GLOBAL_UNIT_ASSIGNED_CONTEXT((#18354,#18356,#18357))
REPRESENTATION_CONTEXT('','3D')
);
#18353=(
GEOMETRIC_REPRESENTATION_CONTEXT(3)
GLOBAL_UNCERTAINTY_ASSIGNED_CONTEXT((#18341))
GLOBAL_UNIT_ASSIGNED_CONTEXT((#18354,#18356,#18357))
REPRESENTATION_CONTEXT('','3D')
);
#18354=(
LENGTH_UNIT()
NAMED_UNIT(*)
SI_UNIT(.CENTI.,.METRE.)
);
#18355=(
LENGTH_UNIT()
NAMED_UNIT(*)
SI_UNIT($,.METRE.)
);
#18356=(
NAMED_UNIT(*)
PLANE_ANGLE_UNIT()
SI_UNIT($,.RADIAN.)
);
#18357=(
NAMED_UNIT(*)
SI_UNIT($,.STERADIAN.)
SOLID_ANGLE_UNIT()
);
#18358=SHAPE_DEFINITION_REPRESENTATION(#18369,#18396);
#18359=SHAPE_DEFINITION_REPRESENTATION(#18370,#18397);
#18360=SHAPE_DEFINITION_REPRESENTATION(#18371,#18398);
#18361=SHAPE_DEFINITION_REPRESENTATION(#18372,#18399);
#18362=SHAPE_DEFINITION_REPRESENTATION(#18373,#18400);
#18363=SHAPE_DEFINITION_REPRESENTATION(#18374,#18401);
#18364=SHAPE_DEFINITION_REPRESENTATION(#18375,#18402);
#18365=SHAPE_DEFINITION_REPRESENTATION(#18376,#18403);
#18366=SHAPE_DEFINITION_REPRESENTATION(#18377,#18404);
#18367=SHAPE_DEFINITION_REPRESENTATION(#18378,#18405);
#18368=SHAPE_DEFINITION_REPRESENTATION(#18387,#18406);
#18369=PRODUCT_DEFINITION_SHAPE('',$,#18408);
#18370=PRODUCT_DEFINITION_SHAPE('',$,#18409);
#18371=PRODUCT_DEFINITION_SHAPE('',$,#18410);
#18372=PRODUCT_DEFINITION_SHAPE('',$,#18411);
#18373=PRODUCT_DEFINITION_SHAPE('',$,#18412);
#18374=PRODUCT_DEFINITION_SHAPE('',$,#18413);
#18375=PRODUCT_DEFINITION_SHAPE('',$,#18414);
#18376=PRODUCT_DEFINITION_SHAPE('',$,#18415);
#18377=PRODUCT_DEFINITION_SHAPE('',$,#18416);
#18378=PRODUCT_DEFINITION_SHAPE('',$,#18417);
#18379=PRODUCT_DEFINITION_SHAPE($,$,#59);
#18380=PRODUCT_DEFINITION_SHAPE($,$,#60);
#18381=PRODUCT_DEFINITION_SHAPE($,$,#61);
#18382=PRODUCT_DEFINITION_SHAPE($,$,#62);
#18383=PRODUCT_DEFINITION_SHAPE($,$,#63);
#18384=PRODUCT_DEFINITION_SHAPE($,$,#64);
#18385=PRODUCT_DEFINITION_SHAPE($,$,#65);
#18386=PRODUCT_DEFINITION_SHAPE($,$,#66);
#18387=PRODUCT_DEFINITION_SHAPE('',$,#18418);
#18388=PRODUCT_DEFINITION_SHAPE($,$,#67);
#18389=PRODUCT_DEFINITION_SHAPE($,$,#68);
#18390=PRODUCT_DEFINITION_SHAPE($,$,#69);
#18391=PRODUCT_DEFINITION_SHAPE($,$,#70);
#18392=PRODUCT_DEFINITION_SHAPE($,$,#71);
#18393=PRODUCT_DEFINITION_SHAPE($,$,#72);
#18394=PRODUCT_DEFINITION_SHAPE($,$,#73);
#18395=PRODUCT_DEFINITION_SHAPE($,$,#74);
#18396=SHAPE_REPRESENTATION('',(#6595,#7074,#7075,#7076,#7077,#7078,#7079,
#7080,#7081),#18342);
#18397=SHAPE_REPRESENTATION('',(#6596),#18343);
#18398=SHAPE_REPRESENTATION('',(#6656),#18344);
#18399=SHAPE_REPRESENTATION('',(#6674),#18345);
#18400=SHAPE_REPRESENTATION('',(#6685,#7057,#7058,#7059,#7060,#7061,#7062,
#7063,#7064),#18346);
#18401=SHAPE_REPRESENTATION('',(#6686),#18347);
#18402=SHAPE_REPRESENTATION('',(#6788),#18348);
#18403=SHAPE_REPRESENTATION('',(#6896),#18349);
#18404=SHAPE_REPRESENTATION('',(#6949),#18350);
#18405=SHAPE_REPRESENTATION('',(#7031),#18351);
#18406=SHAPE_REPRESENTATION('',(#7065),#18352);
#18407=PRODUCT_DEFINITION_CONTEXT('part definition',#18442,'design');
#18408=PRODUCT_DEFINITION('TOOL-020','TOOL-020',#18419,#18407);
#18409=PRODUCT_DEFINITION('Forged jaw and handle',
'Forged jaw and handle',#18420,#18407);
#18410=PRODUCT_DEFINITION('Shoulder pivot pin','Shoulder pivot pin',#18421,
#18407);
#18411=PRODUCT_DEFINITION('Pivot retaining ring','Pivot retaining ring',
#18422,#18407);
#18412=PRODUCT_DEFINITION('Custom handle grip','Custom handle grip',#18423,
#18407);
#18413=PRODUCT_DEFINITION('2026-11-10-01-32-12-355',
'Upper structural shell',#18424,#18407);
#18414=PRODUCT_DEFINITION('2026-11-10-01-32-12-359',
'Lower structural shell',#18425,#18407);
#18415=PRODUCT_DEFINITION('2026-11-10-01-32-12-364','Soft grip layer',#18426,
#18407);
#18416=PRODUCT_DEFINITION('2026-11-10-01-32-12-367',
'Socket head cap screw M3x16',#18427,#18407);
#18417=PRODUCT_DEFINITION('2026-11-10-01-32-12-368','Hex nut M3',#18428,
#18407);
#18418=PRODUCT_DEFINITION('Pivot thrust washer','Pivot thrust washer',#18429,
#18407);
#18419=PRODUCT_DEFINITION_FORMATION('',$,#18444);
#18420=PRODUCT_DEFINITION_FORMATION('',$,#18445);
#18421=PRODUCT_DEFINITION_FORMATION('',$,#18446);
#18422=PRODUCT_DEFINITION_FORMATION('',$,#18447);
#18423=PRODUCT_DEFINITION_FORMATION('',$,#18448);
#18424=PRODUCT_DEFINITION_FORMATION('',$,#18449);
#18425=PRODUCT_DEFINITION_FORMATION('',$,#18450);
#18426=PRODUCT_DEFINITION_FORMATION('',$,#18451);
#18427=PRODUCT_DEFINITION_FORMATION('',$,#18452);
#18428=PRODUCT_DEFINITION_FORMATION('',$,#18453);
#18429=PRODUCT_DEFINITION_FORMATION('',$,#18454);
#18430=PRODUCT_RELATED_PRODUCT_CATEGORY('TOOL-020','TOOL-020',(#18444));
#18431=PRODUCT_RELATED_PRODUCT_CATEGORY('Forged jaw and handle',
'Forged jaw and handle',(#18445));
#18432=PRODUCT_RELATED_PRODUCT_CATEGORY('Shoulder pivot pin',
'Shoulder pivot pin',(#18446));
#18433=PRODUCT_RELATED_PRODUCT_CATEGORY('Pivot retaining ring',
'Pivot retaining ring',(#18447));
#18434=PRODUCT_RELATED_PRODUCT_CATEGORY('Custom handle grip',
'Custom handle grip',(#18448));
#18435=PRODUCT_RELATED_PRODUCT_CATEGORY('Upper structural shell',
'Upper structural shell',(#18449));
#18436=PRODUCT_RELATED_PRODUCT_CATEGORY('Lower structural shell',
'Lower structural shell',(#18450));
#18437=PRODUCT_RELATED_PRODUCT_CATEGORY('Soft grip layer',
'Soft grip layer',(#18451));
#18438=PRODUCT_RELATED_PRODUCT_CATEGORY('Socket head cap screw M3x16',
'Socket head cap screw M3x16',(#18452));
#18439=PRODUCT_RELATED_PRODUCT_CATEGORY('Hex nut M3','Hex nut M3',(#18453));
#18440=PRODUCT_RELATED_PRODUCT_CATEGORY('Pivot thrust washer',
'Pivot thrust washer',(#18454));
#18441=APPLICATION_PROTOCOL_DEFINITION('international standard',
'automotive_design',2009,#18442);
#18442=APPLICATION_CONTEXT(
'Core Data for Automotive Mechanical Design Process');
#18443=PRODUCT_CONTEXT('part definition',#18442,'mechanical');
#18444=PRODUCT('TOOL-020','TOOL-020',$,(#18443));
#18445=PRODUCT('Forged jaw and handle','Forged jaw and handle',$,(#18443));
#18446=PRODUCT('Shoulder pivot pin','Shoulder pivot pin',$,(#18443));
#18447=PRODUCT('Pivot retaining ring','Pivot retaining ring',$,(#18443));
#18448=PRODUCT('Custom handle grip','Custom handle grip',$,(#18443));
#18449=PRODUCT('2026-11-10-01-32-12-355','Upper structural shell',$,(#18443));
#18450=PRODUCT('2026-11-10-01-32-12-359','Lower structural shell',$,(#18443));
#18451=PRODUCT('2026-11-10-01-32-12-364','Soft grip layer',$,(#18443));
#18452=PRODUCT('2026-11-10-01-32-12-367','Socket head cap screw M3x16',
$,(#18443));
#18453=PRODUCT('2026-11-10-01-32-12-368','Hex nut M3',$,(#18443));
#18454=PRODUCT('Pivot thrust washer','Pivot thrust washer',$,(#18443));
#18455=PRESENTATION_STYLE_ASSIGNMENT((#18463));
#18456=PRESENTATION_STYLE_ASSIGNMENT((#18464));
#18457=PRESENTATION_STYLE_ASSIGNMENT((#18465));
#18458=PRESENTATION_STYLE_ASSIGNMENT((#18466));
#18459=PRESENTATION_STYLE_ASSIGNMENT((#18467));
#18460=PRESENTATION_STYLE_ASSIGNMENT((#18468));
#18461=PRESENTATION_STYLE_ASSIGNMENT((#18469));
#18462=PRESENTATION_STYLE_ASSIGNMENT((#18470));
#18463=SURFACE_STYLE_USAGE(.BOTH.,#18471);
#18464=SURFACE_STYLE_USAGE(.BOTH.,#18472);
#18465=SURFACE_STYLE_USAGE(.BOTH.,#18473);
#18466=SURFACE_STYLE_USAGE(.BOTH.,#18474);
#18467=SURFACE_STYLE_USAGE(.BOTH.,#18475);
#18468=SURFACE_STYLE_USAGE(.BOTH.,#18476);
#18469=SURFACE_STYLE_USAGE(.BOTH.,#18477);
#18470=SURFACE_STYLE_USAGE(.BOTH.,#18478);
#18471=SURFACE_SIDE_STYLE('',(#18479));
#18472=SURFACE_SIDE_STYLE('',(#18480));
#18473=SURFACE_SIDE_STYLE('',(#18481));
#18474=SURFACE_SIDE_STYLE('',(#18482));
#18475=SURFACE_SIDE_STYLE('',(#18483));
#18476=SURFACE_SIDE_STYLE('',(#18484));
#18477=SURFACE_SIDE_STYLE('',(#18485));
#18478=SURFACE_SIDE_STYLE('',(#18486));
#18479=SURFACE_STYLE_FILL_AREA(#18487);
#18480=SURFACE_STYLE_FILL_AREA(#18488);
#18481=SURFACE_STYLE_FILL_AREA(#18489);
#18482=SURFACE_STYLE_FILL_AREA(#18490);
#18483=SURFACE_STYLE_FILL_AREA(#18491);
#18484=SURFACE_STYLE_FILL_AREA(#18492);
#18485=SURFACE_STYLE_FILL_AREA(#18493);
#18486=SURFACE_STYLE_FILL_AREA(#18494);
#18487=FILL_AREA_STYLE('Steel - Satin',(#18495));
#18488=FILL_AREA_STYLE('Tool steel gray',(#18496));
#18489=FILL_AREA_STYLE('Pivot dark gray',(#18497));
#18490=FILL_AREA_STYLE('Dark gray',(#18498));
#18491=FILL_AREA_STYLE('Structural dark blue',(#18499));
#18492=FILL_AREA_STYLE('Sky blue soft grip',(#18500));
#18493=FILL_AREA_STYLE('Fastener gray',(#18501));
#18494=FILL_AREA_STYLE('Washer gray',(#18502));
#18495=FILL_AREA_STYLE_COLOUR('Steel - Satin',#18503);
#18496=FILL_AREA_STYLE_COLOUR('Tool steel gray',#18504);
#18497=FILL_AREA_STYLE_COLOUR('Pivot dark gray',#18505);
#18498=FILL_AREA_STYLE_COLOUR('Dark gray',#18506);
#18499=FILL_AREA_STYLE_COLOUR('Structural dark blue',#18507);
#18500=FILL_AREA_STYLE_COLOUR('Sky blue soft grip',#18508);
#18501=FILL_AREA_STYLE_COLOUR('Fastener gray',#18509);
#18502=FILL_AREA_STYLE_COLOUR('Washer gray',#18510);
#18503=COLOUR_RGB('Steel - Satin',0.627450980392157,0.627450980392157,0.627450980392157);
#18504=COLOUR_RGB('Tool steel gray',0.607843137254902,0.643137254901961,
0.698039215686274);
#18505=COLOUR_RGB('Pivot dark gray',0.27843137254902,0.309803921568627,
0.352941176470588);
#18506=COLOUR_RGB('Dark gray',0.250980392156863,0.282352941176471,0.32156862745098);
#18507=COLOUR_RGB('Structural dark blue',0.0901960784313725,0.270588235294118,
0.513725490196078);
#18508=COLOUR_RGB('Sky blue soft grip',0.662745098039216,0.831372549019608,
0.949019607843137);
#18509=COLOUR_RGB('Fastener gray',0.607843137254902,0.643137254901961,0.698039215686274);
#18510=COLOUR_RGB('Washer gray',0.725490196078431,0.752941176470588,0.792156862745098);
ENDSEC;
END-ISO-10303-21;
